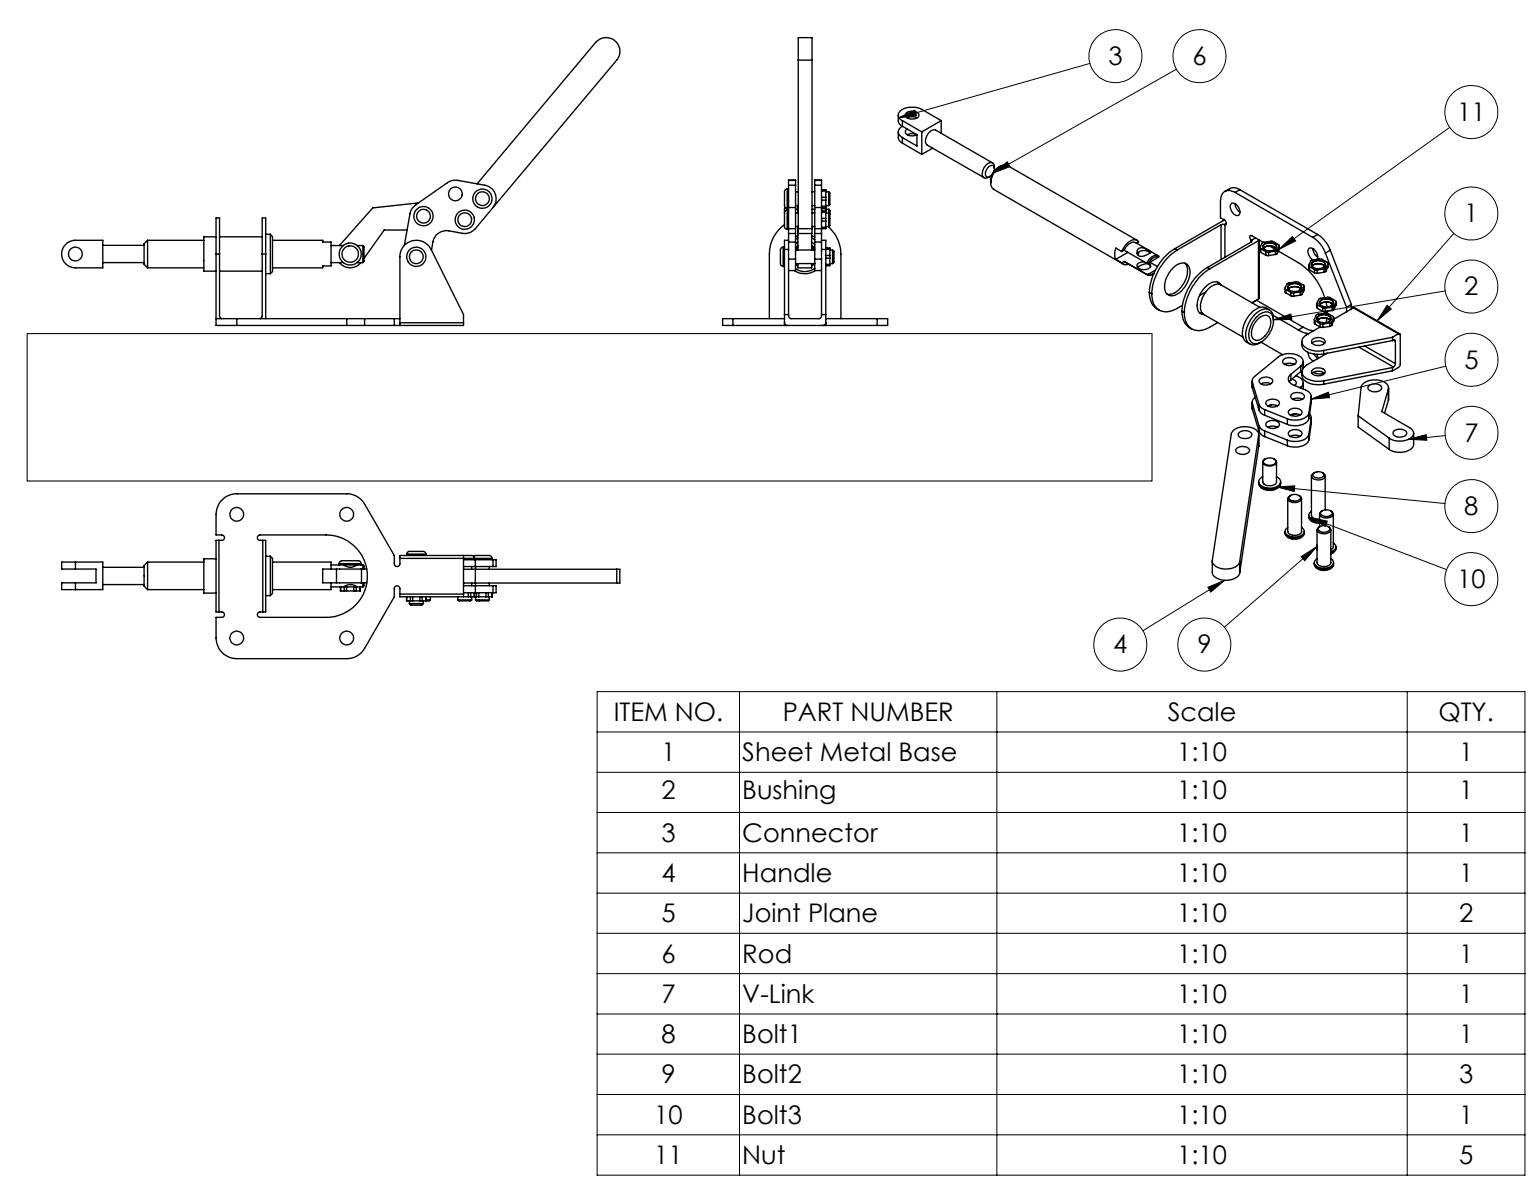
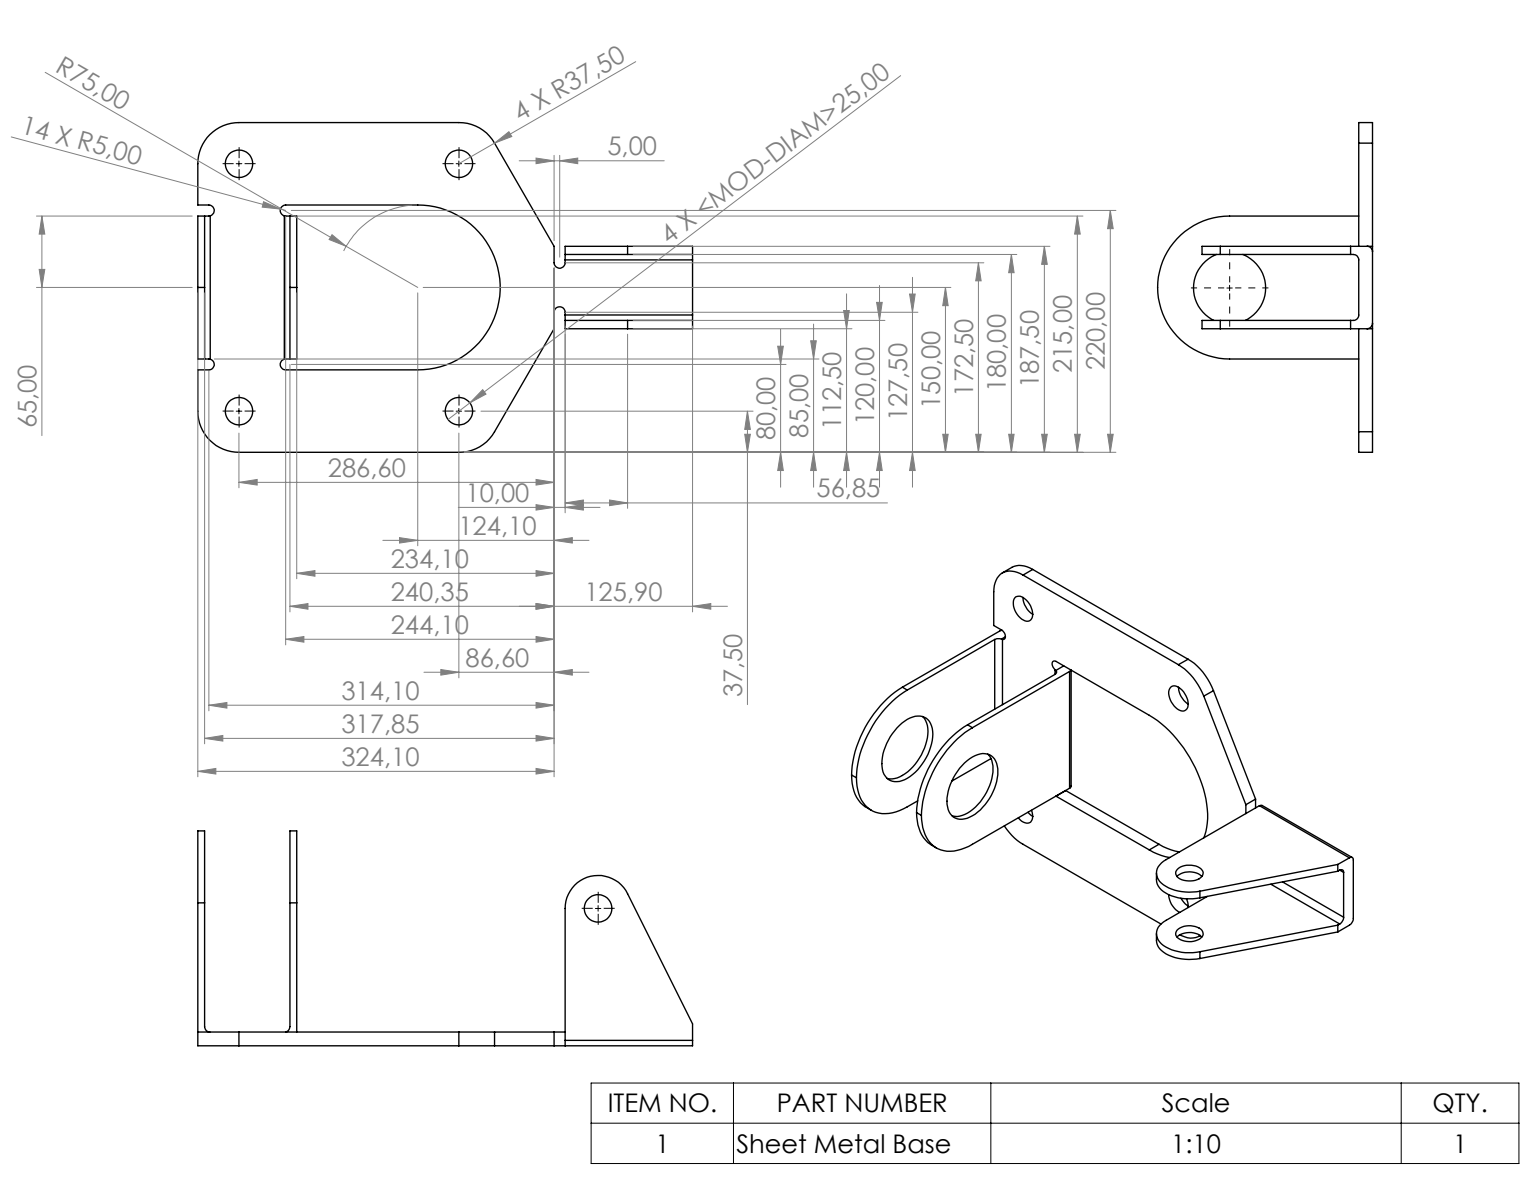
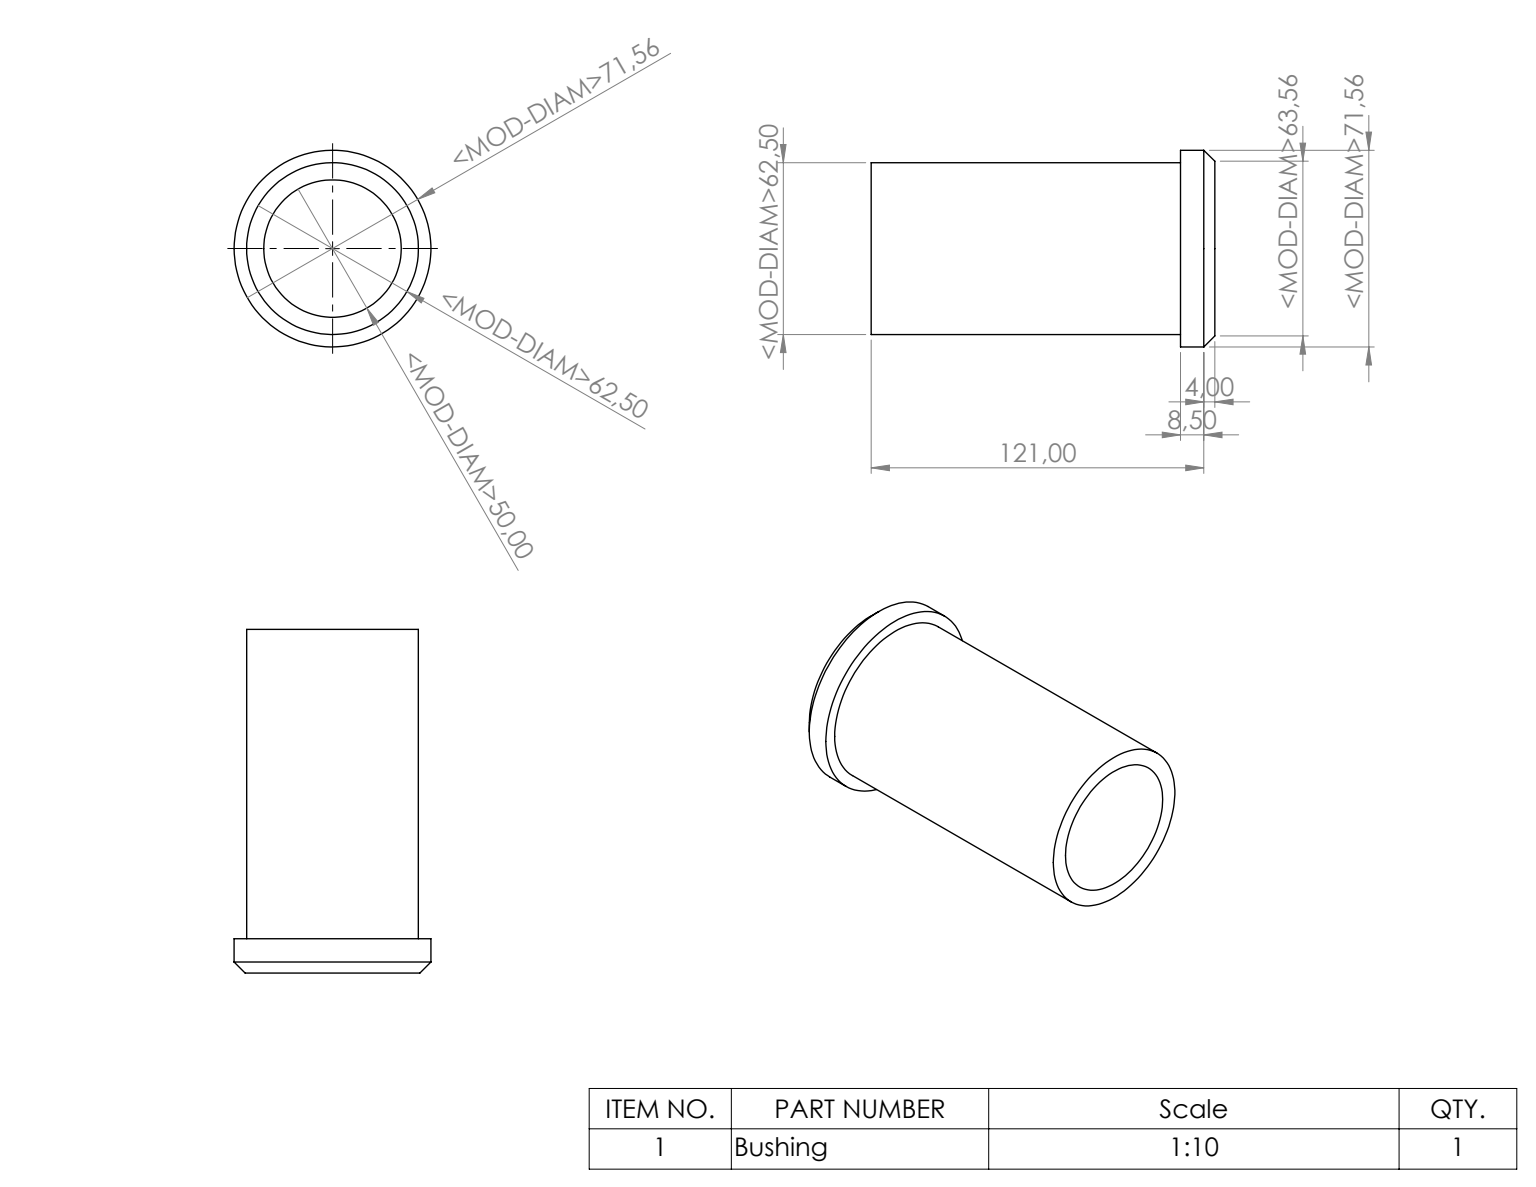
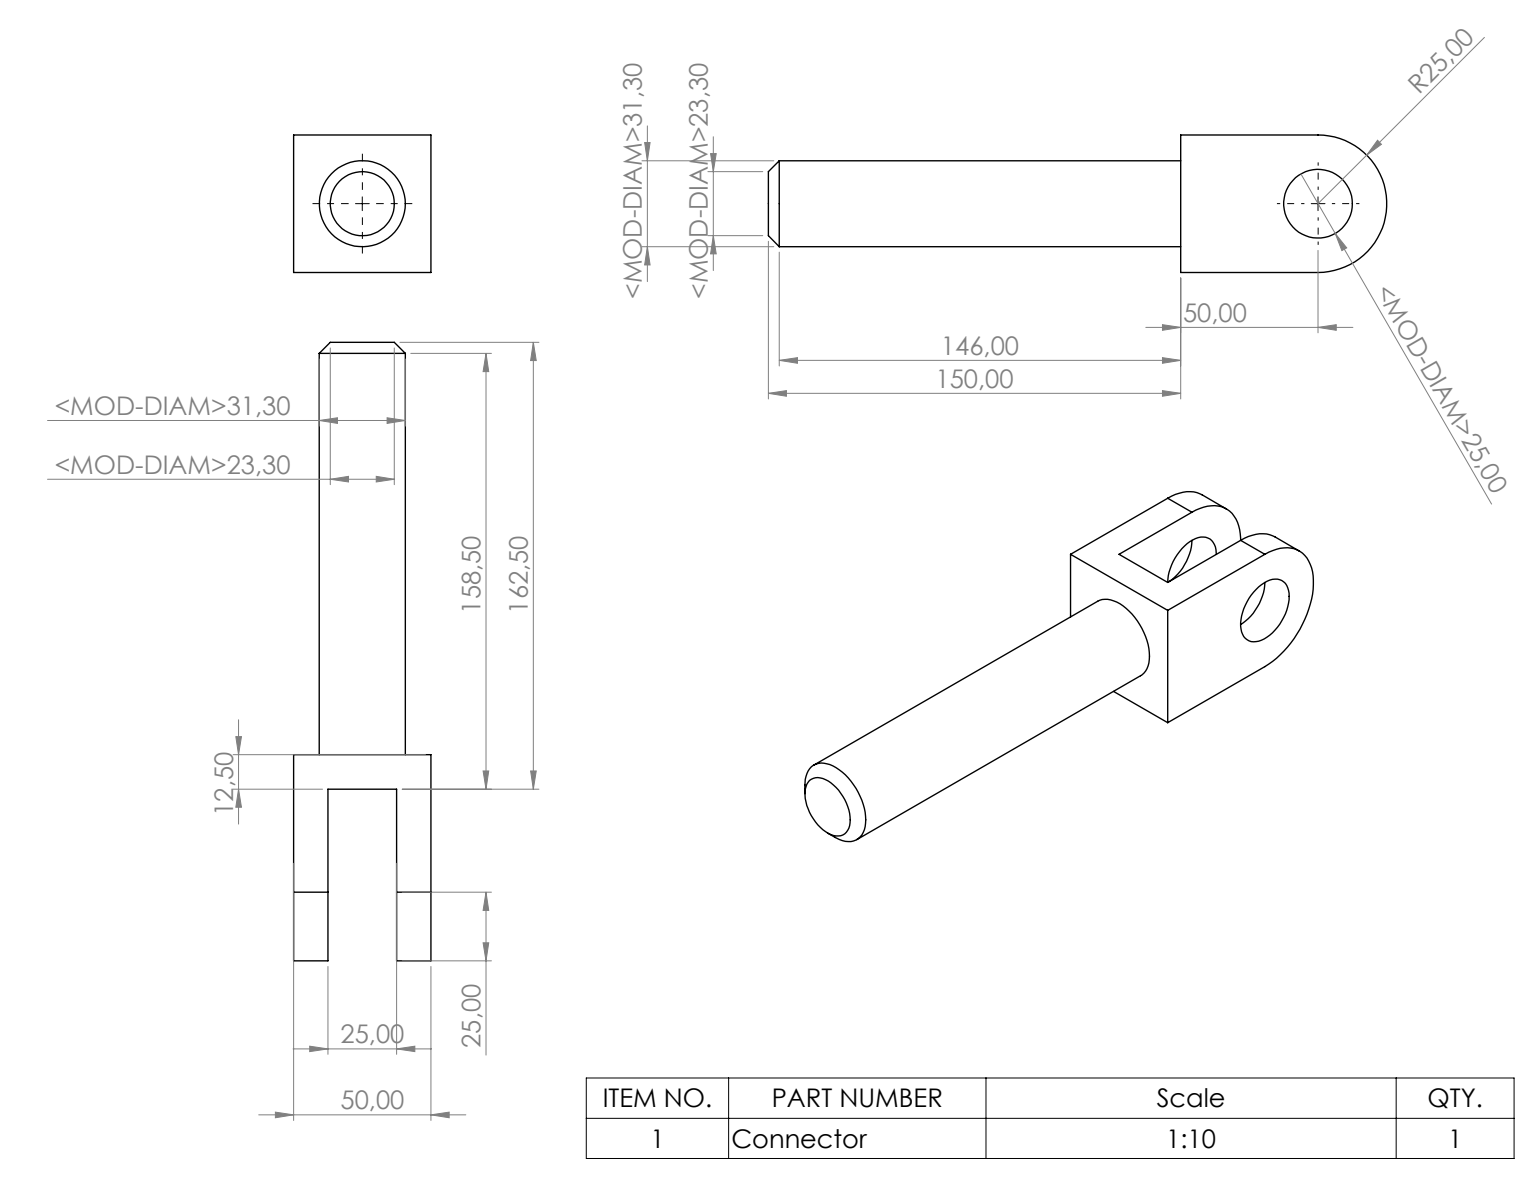
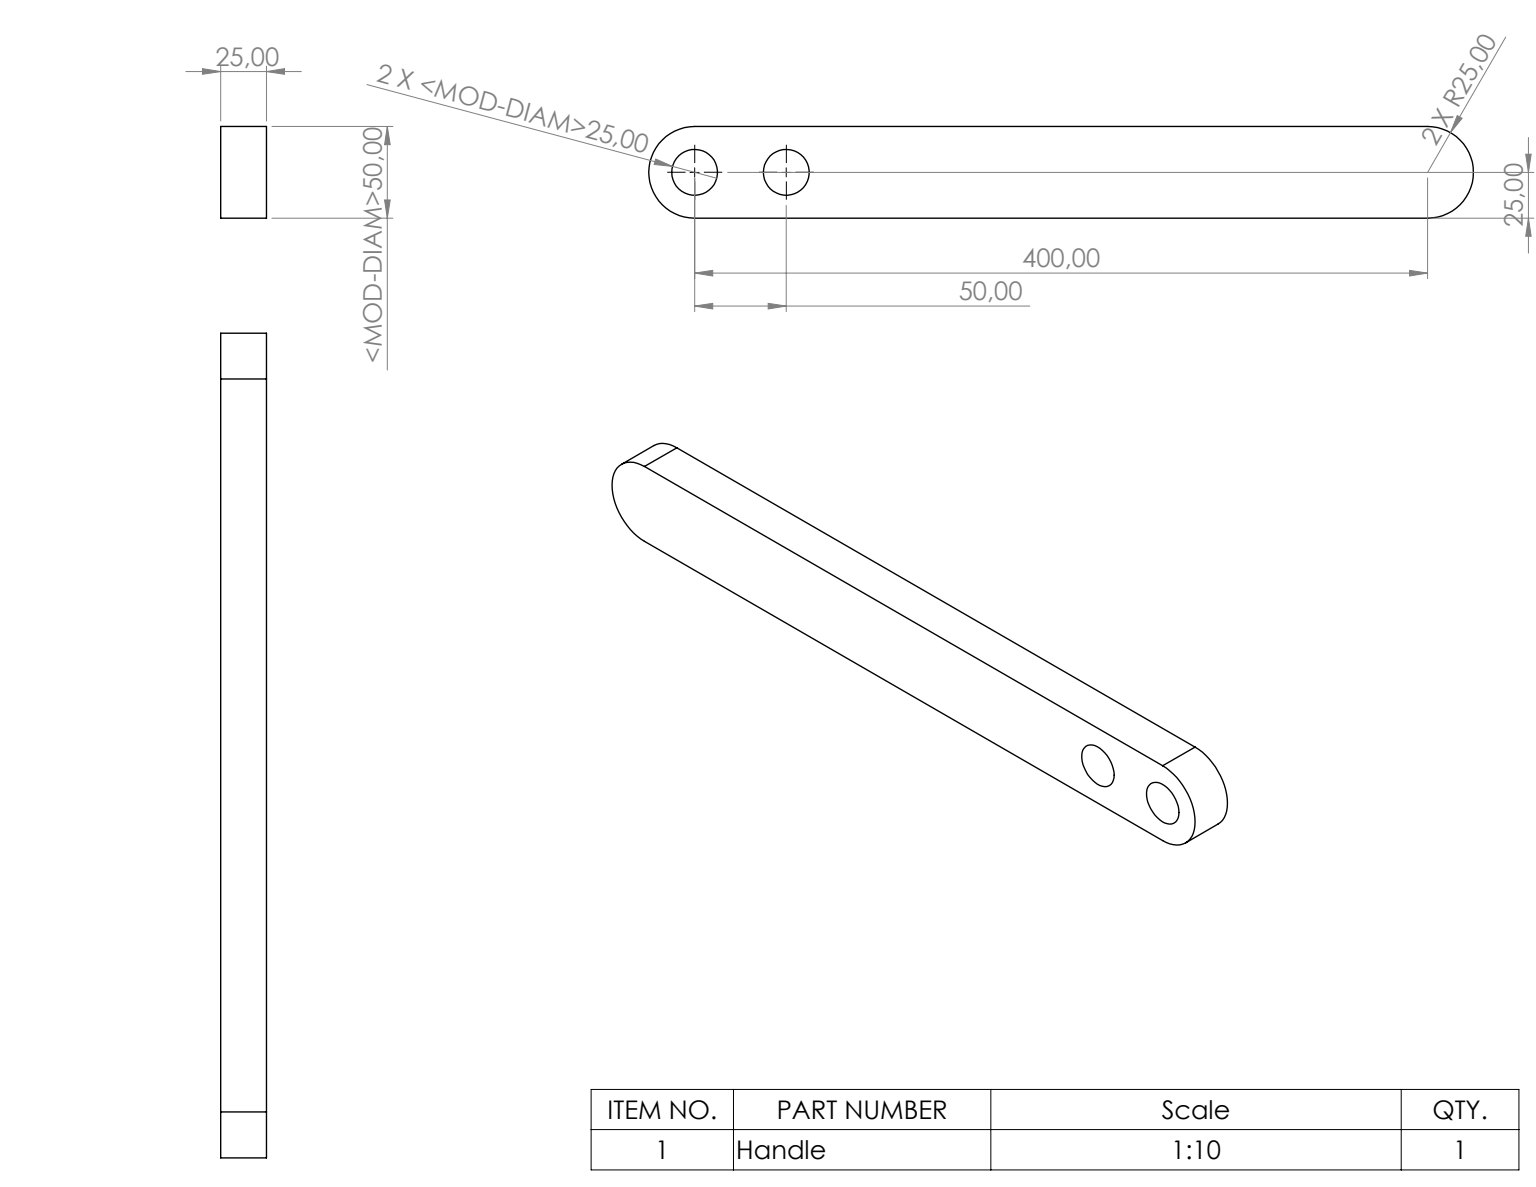
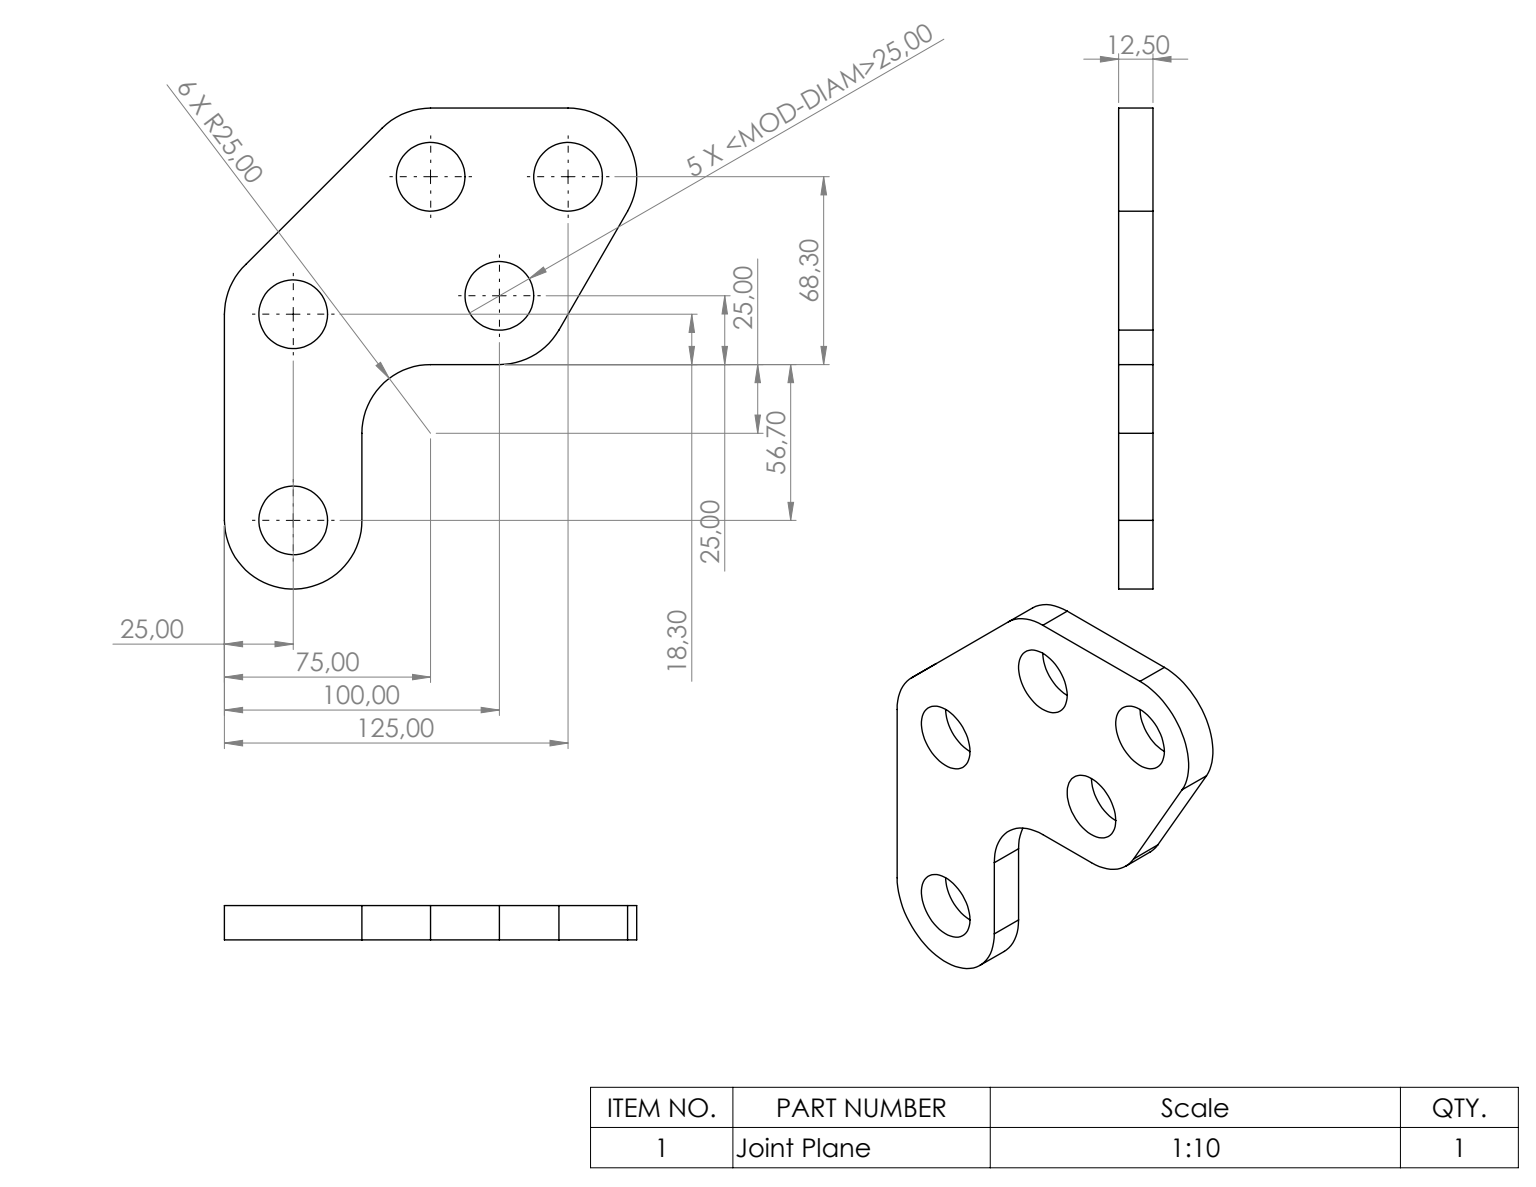
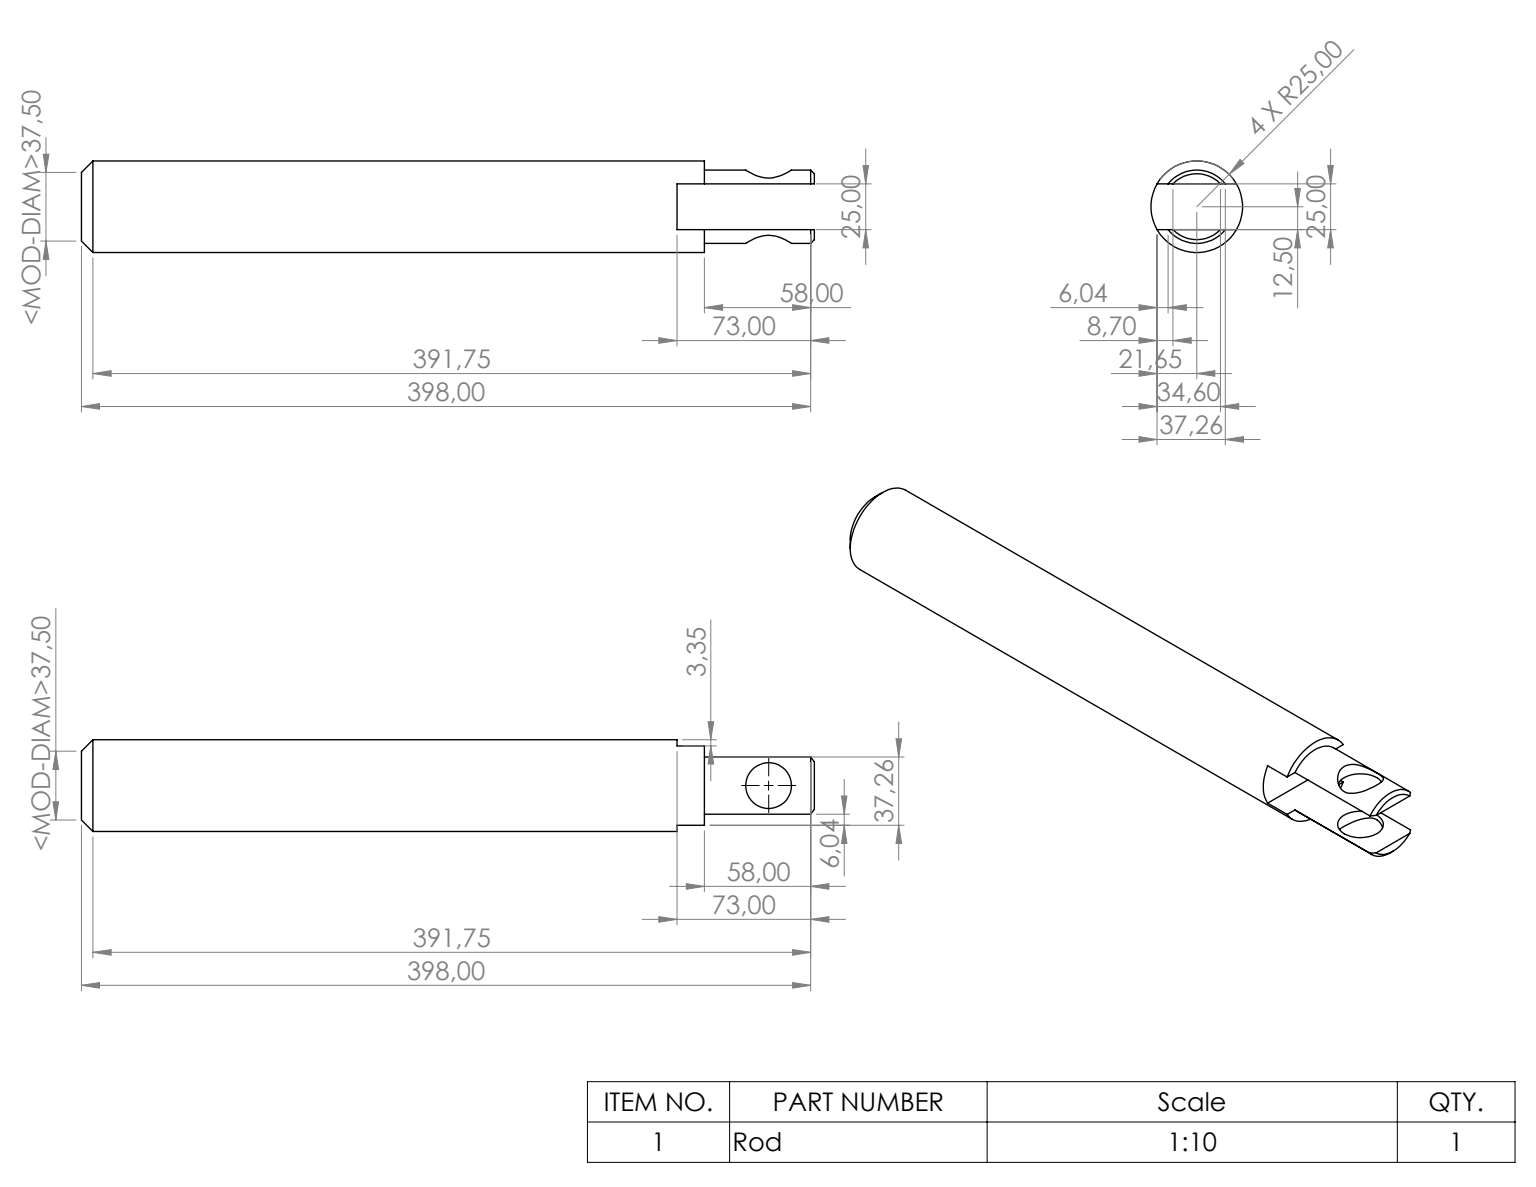
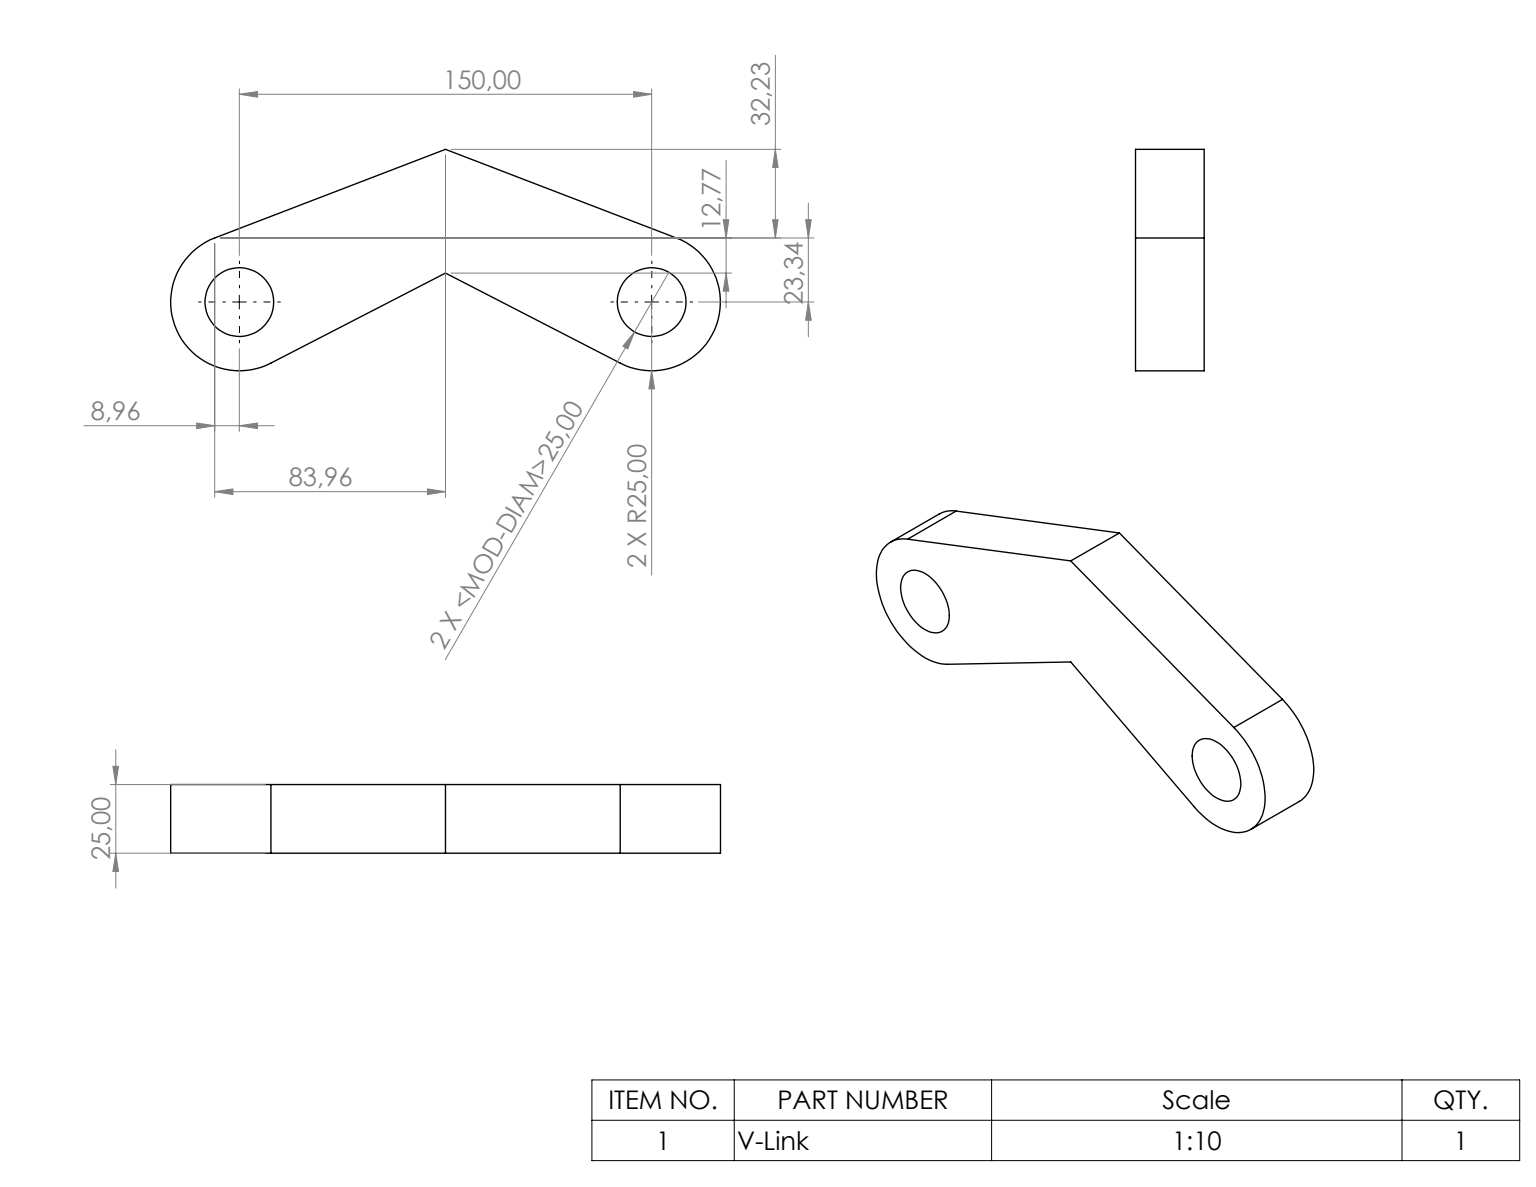
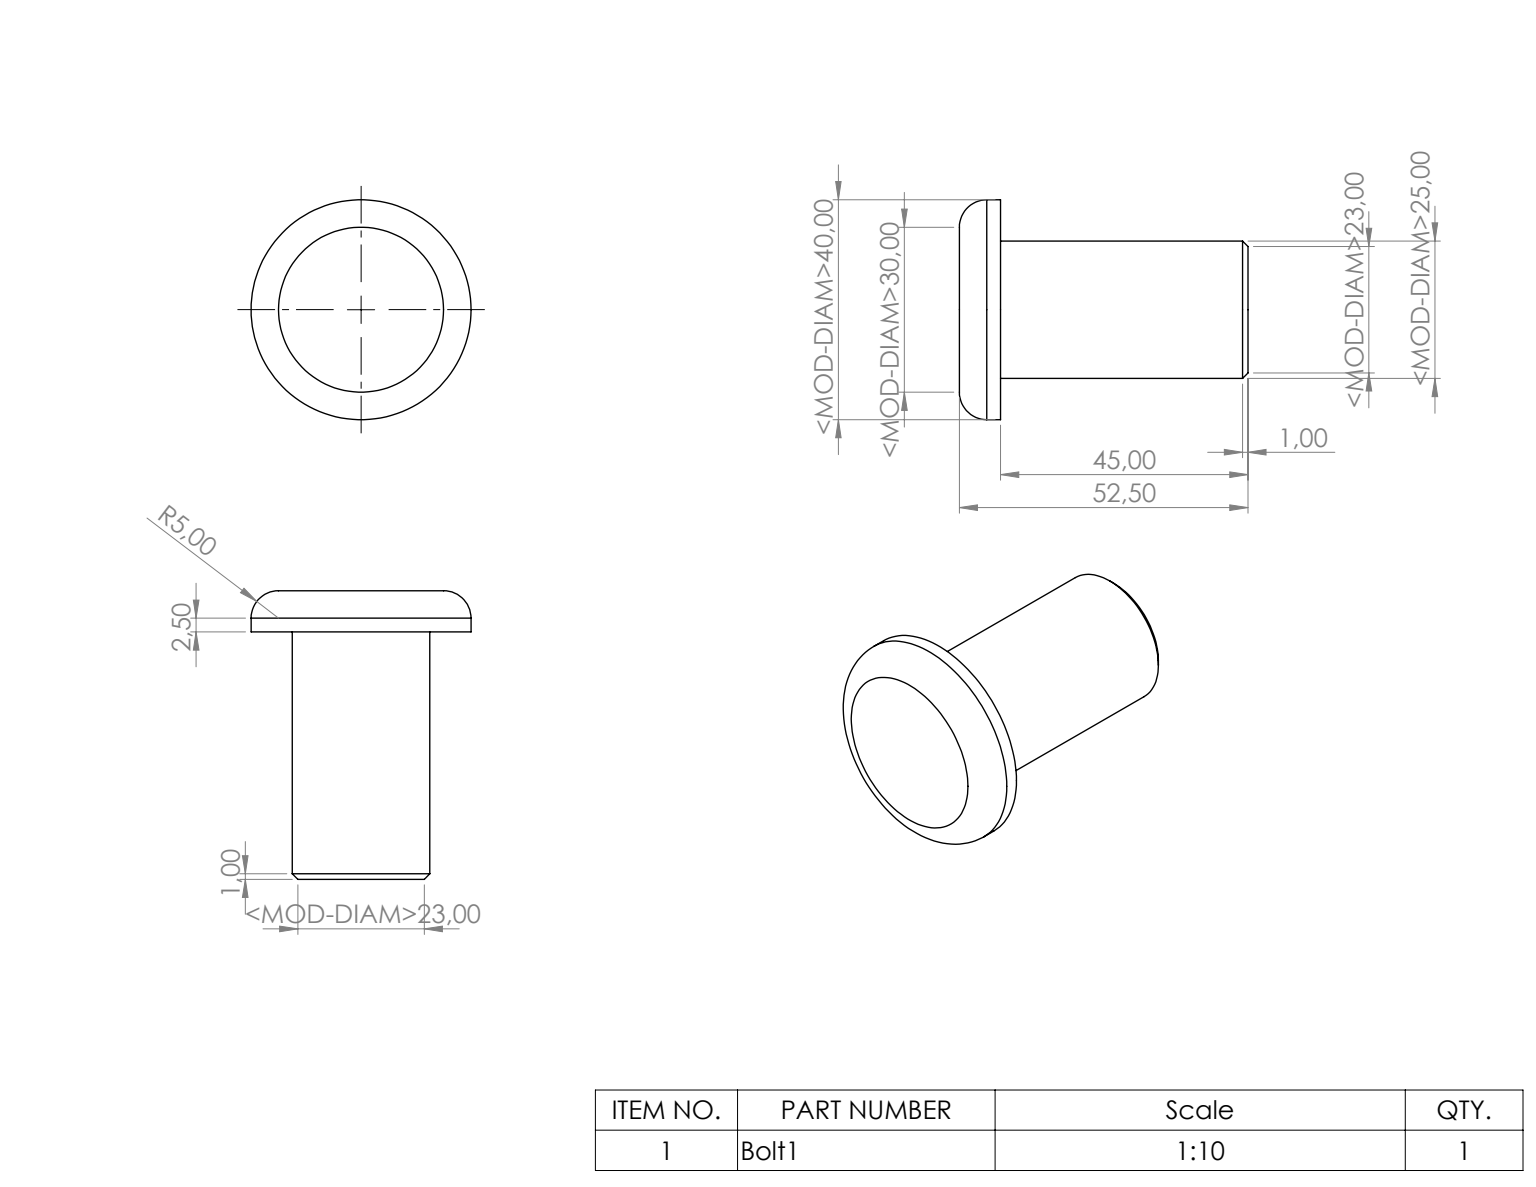
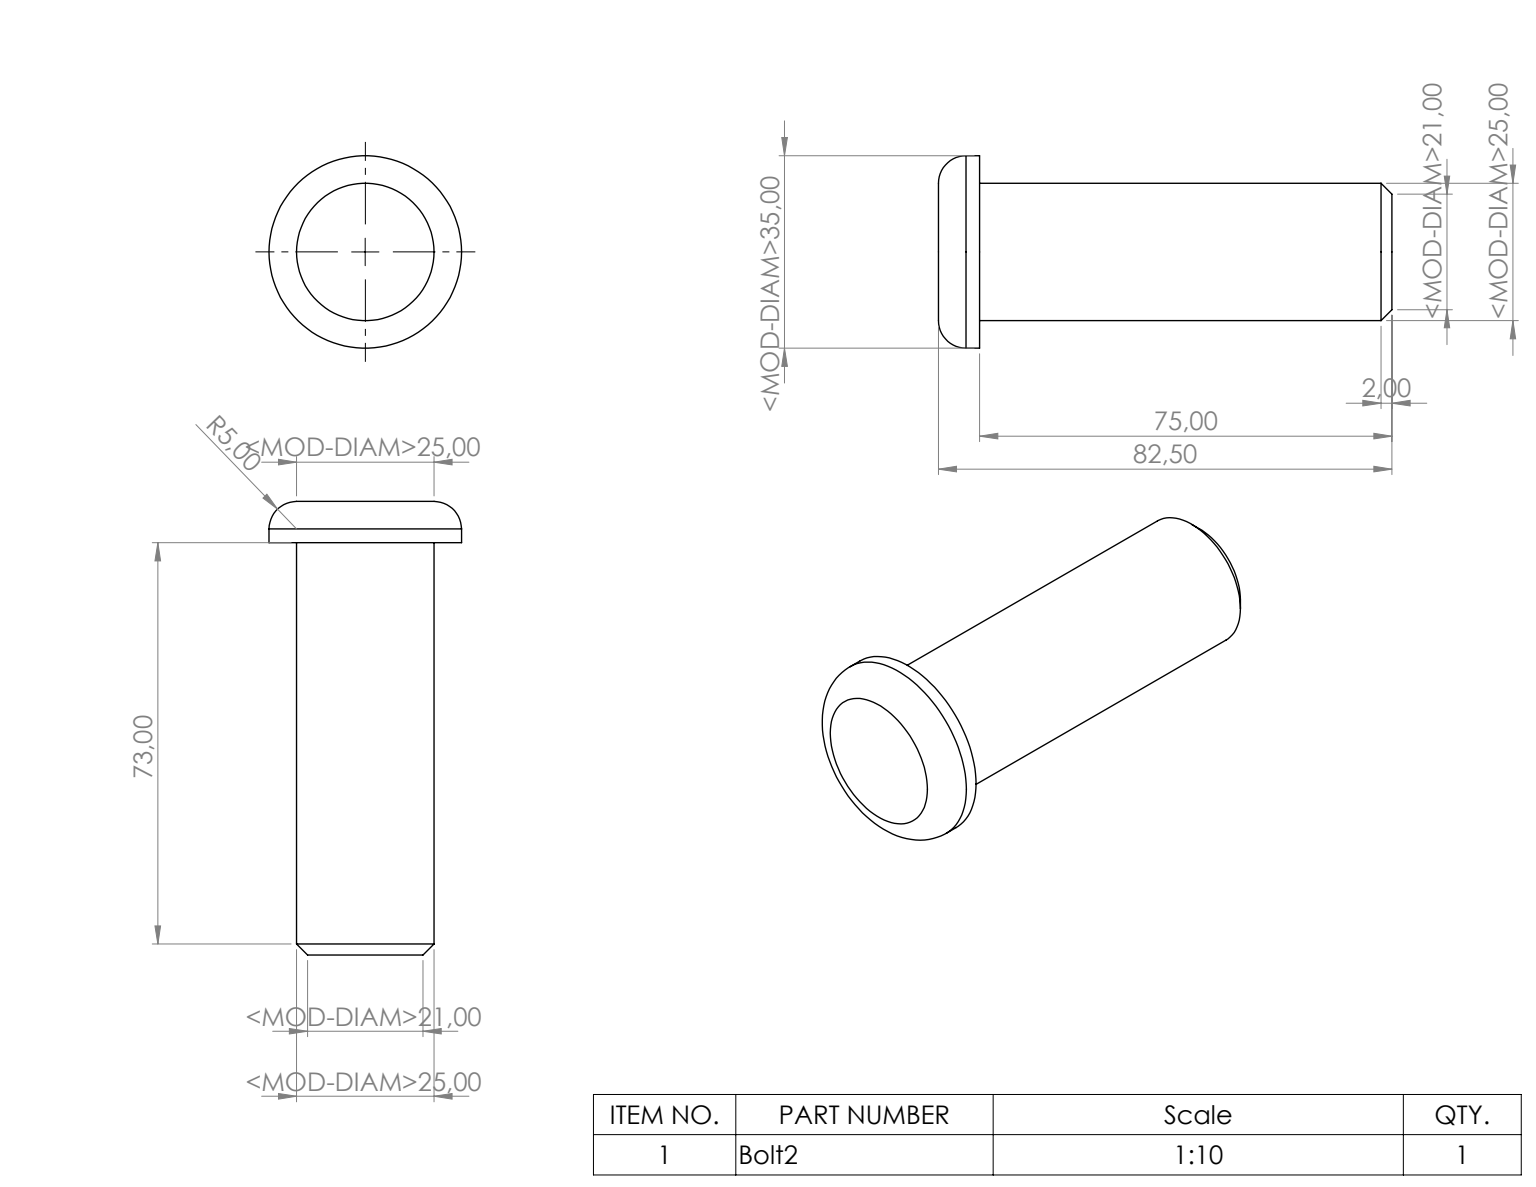
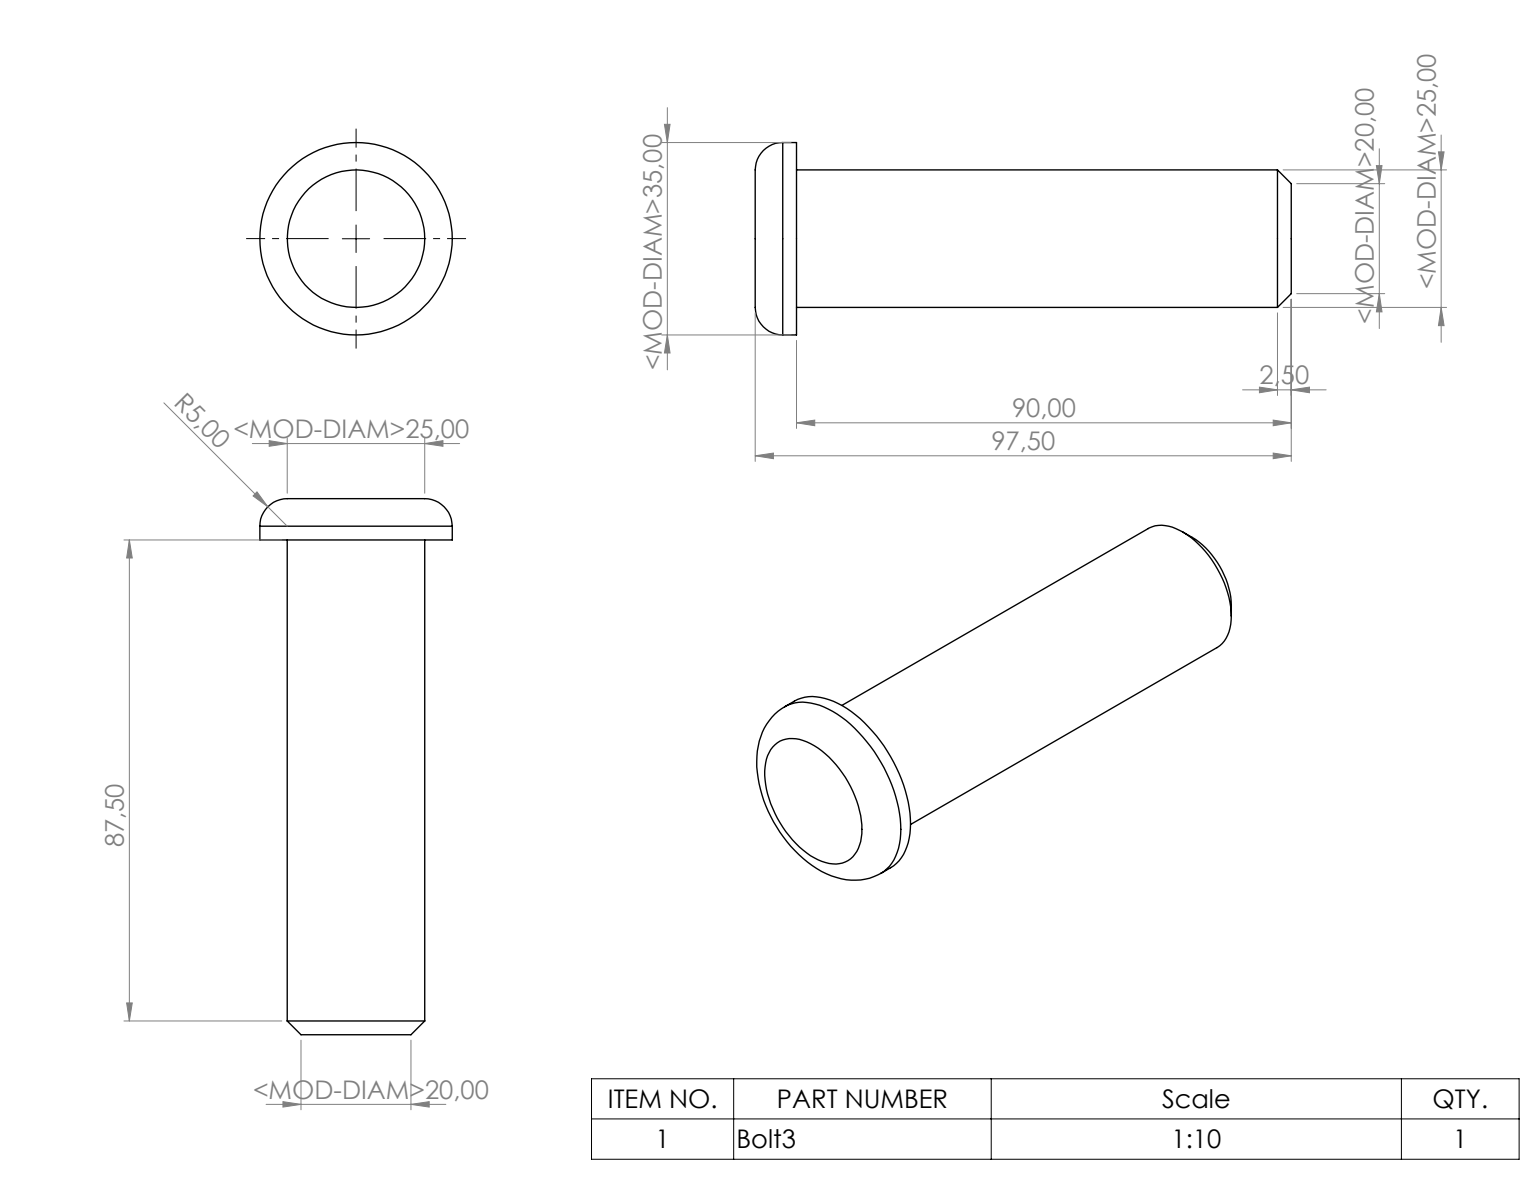
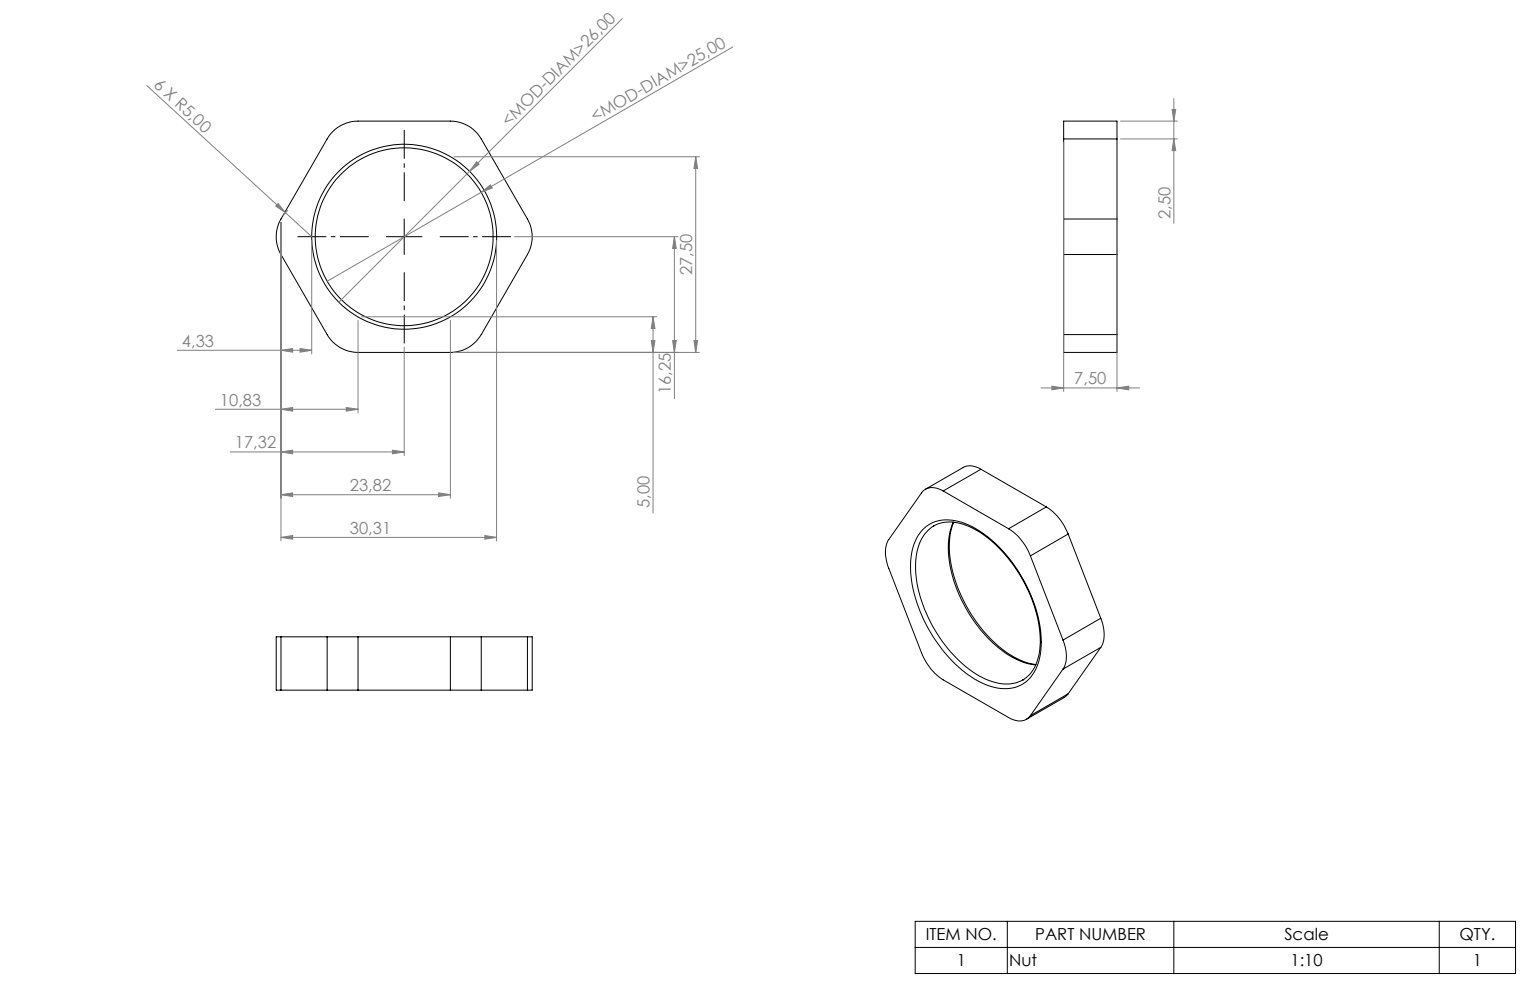
ISO-10303-21;
HEADER;
FILE_DESCRIPTION (('STEP AP214'),
    '1' );
FILE_NAME ('MAT-014',
    '2026-10-28T16:39:03',
    ( '' ),
    ( '' ),
    'SwSTEP 2.0',
    'SolidWorks 2024',
    '' );
FILE_SCHEMA (( 'AUTOMOTIVE_DESIGN' ));
ENDSEC;

DATA;
#1 = VERTEX_POINT ( 'NONE', #6487 ) ;
#2 = VERTEX_POINT ( 'NONE', #3957 ) ;
#3 = CARTESIAN_POINT ( 'NONE',  ( 375.4247212639274380, -15.61249499599598956, 12.50000000000000533 ) ) ;
#4 = ADVANCED_FACE ( 'NONE', ( #7050 ), #2111, .F. ) ;
#5 = LINE ( 'NONE', #7463, #3697 ) ;
#6 = DIRECTION ( 'NONE',  ( 1.000000000000000000, 0.000000000000000000, 0.000000000000000000 ) ) ;
#7 = LINE ( 'NONE', #3105, #4260 ) ;
#8 = CARTESIAN_POINT ( 'NONE',  ( 3.081487911019577803E-31, -25.00000000000000355, 37.50000000000000000 ) ) ;
#9 = CARTESIAN_POINT ( 'NONE',  ( 387.3898630172379285, 19.93132096080314497, 1.708129828930195826 ) ) ;
#10 = ADVANCED_BREP_SHAPE_REPRESENTATION ( '', ( #4174, #5785 ), #5126 ) ;
#11 = LINE ( 'NONE', #7275, #2680 ) ;
#12 = AXIS2_PLACEMENT_3D ( 'NONE', #2676, #866, #3439 ) ;
#13 = DIRECTION ( 'NONE',  ( -1.000000000000000000, -0.000000000000000000, -0.000000000000000000 ) ) ;
#14 = CARTESIAN_POINT ( 'NONE',  ( -12.99038105676657651, 1.734723475976807094E-15, 0.000000000000000000 ) ) ;
#15 = CARTESIAN_POINT ( 'NONE',  ( 199.9999999999998863, 262.5000000000000568, 0.000000000000000000 ) ) ;
#16 = AXIS2_PLACEMENT_3D ( 'NONE', #4137, #1054, #5872 ) ;
#17 = ORIENTED_EDGE ( 'NONE', *, *, #7884, .F. ) ;
#18 = ORIENTED_EDGE ( 'NONE', *, *, #3876, .T. ) ;
#19 = LINE ( 'NONE', #1821, #4426 ) ;
#20 = DIRECTION ( 'NONE',  ( 1.000000000000000000, 0.000000000000000000, 0.000000000000000000 ) ) ;
#21 = DIRECTION ( 'NONE',  ( 0.000000000000000000, 0.000000000000000000, -1.000000000000000000 ) ) ;
#22 = EDGE_LOOP ( 'NONE', ( #4827, #5476, #5226, #672 ) ) ;
#23 = CARTESIAN_POINT ( 'NONE',  ( -74.28095588234631919, 12.70544120911856112, 12.50000000000000000 ) ) ;
#24 = ADVANCED_FACE ( 'NONE', ( #907 ), #1513, .T. ) ;
#25 = ORIENTED_EDGE ( 'NONE', *, *, #6041, .T. ) ;
#26 = ADVANCED_FACE ( 'NONE', ( #6325 ), #4629, .T. ) ;
#27 = CARTESIAN_POINT ( 'NONE',  ( 371.6961001703501211, 15.95358756117676258, -12.06260739558933714 ) ) ;
#28 = VERTEX_POINT ( 'NONE', #2799 ) ;
#29 = CARTESIAN_POINT ( 'NONE',  ( 368.6956339375703351, -16.83403191367835561, 10.80131548116625417 ) ) ;
#30 = VERTEX_POINT ( 'NONE', #1471 ) ;
#31 = LINE ( 'NONE', #3054, #2794 ) ;
#32 = DIRECTION ( 'NONE',  ( 1.000000000000000000, 0.000000000000000000, 0.000000000000000000 ) ) ;
#33 = EDGE_CURVE ( 'NONE', #7631, #7527, #437, .T. ) ;
#34 = ORIENTED_EDGE ( 'NONE', *, *, #3876, .F. ) ;
#35 = EDGE_LOOP ( 'NONE', ( #6541, #2279, #2364, #4470, #5618 ) ) ;
#36 = VERTEX_POINT ( 'NONE', #5235 ) ;
#37 = CARTESIAN_POINT ( 'NONE',  ( 376.6870407283136046, -15.69785030319133945, 12.39275847443047773 ) ) ;
#38 = CARTESIAN_POINT ( 'NONE',  ( 0.000000000000000000, 0.000000000000000000, 75.00000000000000000 ) ) ;
#39 = DIRECTION ( 'NONE',  ( 1.000000000000000000, 0.000000000000000000, 0.000000000000000000 ) ) ;
#40 = LINE ( 'NONE', #6225, #5683 ) ;
#41 = DIRECTION ( 'NONE',  ( 0.000000000000000000, -1.000000000000000000, 0.000000000000000000 ) ) ;
#42 = CIRCLE ( 'NONE', #1071, 15.64999999999999680 ) ;
#43 = EDGE_CURVE ( 'NONE', #2392, #5200, #812, .T. ) ;
#44 = VECTOR ( 'NONE', #6723, 1000.000000000000000 ) ;
#45 = AXIS2_PLACEMENT_3D ( 'NONE', #6354, #218, #7634 ) ;
#46 = DIRECTION ( 'NONE',  ( 0.7071067811865502373, 0.000000000000000000, 0.7071067811865447972 ) ) ;
#47 = CARTESIAN_POINT ( 'NONE',  ( -24.28095581706361727, -30.59582894744887582, 0.000000000000000000 ) ) ;
#48 = FACE_OUTER_BOUND ( 'NONE', #2158, .T. ) ;
#49 = DIRECTION ( 'NONE',  ( 0.000000000000000000, 0.000000000000000000, 1.000000000000000000 ) ) ;
#50 = AXIS2_PLACEMENT_3D ( 'NONE', #3727, #3599, #6048 ) ;
#51 = AXIS2_PLACEMENT_3D ( 'NONE', #3862, #3896, #3257 ) ;
#52 = VERTEX_POINT ( 'NONE', #7725 ) ;
#53 = ORIENTED_EDGE ( 'NONE', *, *, #7404, .F. ) ;
#54 = LINE ( 'NONE', #4948, #4837 ) ;
#56 = CARTESIAN_POINT ( 'NONE',  ( 0.7190441502950353225, 87.70544117646394966, 0.000000000000000000 ) ) ;
#55 = CIRCLE ( 'NONE', #4287, 65.50000000000000000 ) ;
#57 = AXIS2_PLACEMENT_3D ( 'NONE', #6318, #3273, #5723 ) ;
#58 = DIRECTION ( 'NONE',  ( 1.000000000000000000, 0.000000000000000000, 0.000000000000000000 ) ) ;
#59 = ORIENTED_EDGE ( 'NONE', *, *, #2376, .F. ) ;
#60 = DIRECTION ( 'NONE',  ( 0.000000000000000000, -0.000000000000000000, 1.000000000000000000 ) ) ;
#61 = ADVANCED_FACE ( 'NONE', ( #3280, #3358 ), #6366, .T. ) ;
#62 = AXIS2_PLACEMENT_3D ( 'NONE', #1310, #5647, #5485 ) ;
#63 = ORIENTED_EDGE ( 'NONE', *, *, #3507, .F. ) ;
#64 = CARTESIAN_POINT ( 'NONE',  ( 370.5187250548066231, 16.23897639391231706, -11.67616422689687639 ) ) ;
#65 = ORIENTED_EDGE ( 'NONE', *, *, #7166, .T. ) ;
#66 = CARTESIAN_POINT ( 'NONE',  ( 364.2065580935995968, -18.97653311414304511, 6.355249004872655760 ) ) ;
#67 = ORIENTED_EDGE ( 'NONE', *, *, #5175, .F. ) ;
#68 = EDGE_CURVE ( 'NONE', #6240, #2057, #7224, .T. ) ;
#69 = CARTESIAN_POINT ( 'NONE',  ( 0.000000000000000000, 0.000000000000000000, 0.000000000000000000 ) ) ;
#70 = VECTOR ( 'NONE', #486, 999.9999999999998863 ) ;
#71 = DIRECTION ( 'NONE',  ( -0.000000000000000000, -0.000000000000000000, -1.000000000000000000 ) ) ;
#72 = EDGE_CURVE ( 'NONE', #4343, #3684, #1276, .T. ) ;
#73 = ORIENTED_EDGE ( 'NONE', *, *, #3667, .F. ) ;
#74 = ORIENTED_EDGE ( 'NONE', *, *, #3629, .F. ) ;
#75 = B_SPLINE_CURVE_WITH_KNOTS ( 'NONE', 3,
 ( #2455, #1205, #4890, #7349 ),
 .UNSPECIFIED., .F., .F.,
 ( 4, 4 ),
 ( 0.000000000000000000, 0.001270006434950045771 ),
 .UNSPECIFIED. ) ;
#76 = EDGE_CURVE ( 'NONE', #6360, #3593, #5967, .T. ) ;
#77 = ORIENTED_EDGE ( 'NONE', *, *, #5334, .F. ) ;
#78 = CARTESIAN_POINT ( 'NONE',  ( 1.320471425210250835E-15, 0.000000000000000000, 0.000000000000000000 ) ) ;
#79 = ADVANCED_FACE ( 'NONE', ( #5146 ), #2881, .F. ) ;
#80 = LINE ( 'NONE', #2529, #4060 ) ;
#81 = CARTESIAN_POINT ( 'NONE',  ( 279.9038105676658006, 161.6025403784438765, 0.000000000000000000 ) ) ;
#82 = FACE_OUTER_BOUND ( 'NONE', #3199, .T. ) ;
#83 = CARTESIAN_POINT ( 'NONE',  ( 25.71904415029483459, 19.40417101989674009, 12.50000000000000000 ) ) ;
#84 = PRESENTATION_LAYER_ASSIGNMENT (  '', '', ( #3420 ) ) ;
#85 = EDGE_CURVE ( 'NONE', #4850, #1396, #297, .T. ) ;
#86 = VECTOR ( 'NONE', #7226, 1000.000000000000000 ) ;
#87 = SHAPE_DEFINITION_REPRESENTATION ( #2063, #2908 ) ;
#88 = CARTESIAN_POINT ( 'NONE',  ( 47.36967921662626679, 6.904171036223937463, 0.000000000000000000 ) ) ;
#89 = DIRECTION ( 'NONE',  ( -0.000000000000000000, -0.000000000000000000, -1.000000000000000000 ) ) ;
#90 = DIRECTION ( 'NONE',  ( -0.000000000000000000, -0.000000000000000000, -1.000000000000000000 ) ) ;
#91 = CYLINDRICAL_SURFACE ( 'NONE', #5688, 5.000000000000004441 ) ;
#92 = CIRCLE ( 'NONE', #7022, 0.5000000000000004441 ) ;
#93 = EDGE_LOOP ( 'NONE', ( #2797, #6100, #4748, #419 ) ) ;
#94 =( LENGTH_UNIT ( ) NAMED_UNIT ( * ) SI_UNIT ( .MILLI., .METRE. ) );
#95 = ORIENTED_EDGE ( 'NONE', *, *, #1155, .F. ) ;
#96 = COLOUR_RGB ( '',0.7921568627450980005, 0.8196078431372548767, 0.9333333333333333481 ) ;
#97 = DIRECTION ( 'NONE',  ( 0.5000000000000000000, 0.8660254037844385966, 0.000000000000000000 ) ) ;
#98 = CYLINDRICAL_SURFACE ( 'NONE', #6896, 12.50000000000001066 ) ;
#99 = CIRCLE ( 'NONE', #3701, 12.50000000000001066 ) ;
#100 = PLANE ( 'NONE',  #441 ) ;
#101 = EDGE_CURVE ( 'NONE', #792, #1942, #1186, .T. ) ;
#102 = FACE_OUTER_BOUND ( 'NONE', #3804, .T. ) ;
#103 = VERTEX_POINT ( 'NONE', #2394 ) ;
#104 = CARTESIAN_POINT ( 'NONE',  ( 0.000000000000000000, 187.5000000000000000, 0.000000000000000000 ) ) ;
#105 = VECTOR ( 'NONE', #3844, 1000.000000000000000 ) ;
#106 = VECTOR ( 'NONE', #6998, 1000.000000000000000 ) ;
#107 = VERTEX_POINT ( 'NONE', #1630 ) ;
#108 = LINE ( 'NONE', #6772, #1142 ) ;
#109 = VERTEX_POINT ( 'NONE', #3635 ) ;
#110 = CARTESIAN_POINT ( 'NONE',  ( -13.00000000000000178, 1.592040838891559293E-15, 7.500000000000000000 ) ) ;
#111 = ORIENTED_EDGE ( 'NONE', *, *, #2037, .T. ) ;
#112 = VECTOR ( 'NONE', #5302, 1000.000000000000000 ) ;
#113 = DIRECTION ( 'NONE',  ( 0.000000000000000000, 0.000000000000000000, 1.000000000000000000 ) ) ;
#114 = AXIS2_PLACEMENT_3D ( 'NONE', #4743, #7238, #7119 ) ;
#115 = LINE ( 'NONE', #7340, #7495 ) ;
#116 = VERTEX_POINT ( 'NONE', #2354 ) ;
#117 = VECTOR ( 'NONE', #1190, 1000.000000000000000 ) ;
#118 = CIRCLE ( 'NONE', #4338, 5.000000000000000888 ) ;
#119 = EDGE_LOOP ( 'NONE', ( #1348, #4627 ) ) ;
#120 = ORIENTED_EDGE ( 'NONE', *, *, #43, .F. ) ;
#121 = CARTESIAN_POINT ( 'NONE',  ( 10.82531754730547213, 13.75000000000000178, 7.500000000000000000 ) ) ;
#122 = CARTESIAN_POINT ( 'NONE',  ( 375.8519756245596568, -15.61249499599599311, -12.50000000000000000 ) ) ;
#123 = DIRECTION ( 'NONE',  ( 1.000000000000000000, 0.000000000000000000, 0.000000000000000000 ) ) ;
#124 = DIRECTION ( 'NONE',  ( -1.000000000000000000, 0.000000000000000000, 0.000000000000000000 ) ) ;
#125 = CYLINDRICAL_SURFACE ( 'NONE', #7742, 12.50000000000000000 ) ;
#126 = EDGE_CURVE ( 'NONE', #36, #6483, #6084, .T. ) ;
#127 = EDGE_CURVE ( 'NONE', #5728, #5686, #5812, .T. ) ;
#128 = CONTEXT_DEPENDENT_SHAPE_REPRESENTATION ( #3628, #4558 ) ;
#129 = CARTESIAN_POINT ( 'NONE',  ( 42.50000000000000000, 42.50000000000003553, 12.50000000000000000 ) ) ;
#130 = CARTESIAN_POINT ( 'NONE',  ( 72.36967921662629522, 50.20544122544588816, 12.50000000000000000 ) ) ;
#131 = LINE ( 'NONE', #1259, #5311 ) ;
#132 = CARTESIAN_POINT ( 'NONE',  ( 125.0000000000000000, 0.000000000000000000, 0.000000000000000000 ) ) ;
#133 = APPLICATION_CONTEXT ( 'automotive_design' ) ;
#134 = EDGE_CURVE ( 'NONE', #6179, #1386, #5939, .T. ) ;
#135 = ADVANCED_FACE ( 'NONE', ( #1032 ), #5362, .T. ) ;
#136 = VERTEX_POINT ( 'NONE', #4752 ) ;
#137 = CARTESIAN_POINT ( 'NONE',  ( 6.495190528383280260, 11.25000000000000000, 7.500000000000000000 ) ) ;
#138 = ORIENTED_EDGE ( 'NONE', *, *, #4119, .T. ) ;
#139 = CYLINDRICAL_SURFACE ( 'NONE', #3161, 24.99999999999999289 ) ;
#140 = DIRECTION ( 'NONE',  ( -0.000000000000000000, -0.000000000000000000, -1.000000000000000000 ) ) ;
#141 = DIRECTION ( 'NONE',  ( -0.000000000000000000, 0.000000000000000000, 1.000000000000000000 ) ) ;
#142 = CARTESIAN_POINT ( 'NONE',  ( -31.24999999999997158, 111.9999999999999289, 130.0000000000000000 ) ) ;
#143 = ORIENTED_EDGE ( 'NONE', *, *, #3611, .T. ) ;
#144 = VECTOR ( 'NONE', #7565, 1000.000000000000000 ) ;
#145 = DIRECTION ( 'NONE',  ( -0.000000000000000000, -0.000000000000000000, -1.000000000000000000 ) ) ;
#146 = VECTOR ( 'NONE', #1608, 1000.000000000000000 ) ;
#147 = EDGE_CURVE ( 'NONE', #3810, #7620, #42, .T. ) ;
#148 = CARTESIAN_POINT ( 'NONE',  ( 362.5886599408613051, 19.94427247194493802, -1.702902647306309358 ) ) ;
#150 = VERTEX_POINT ( 'NONE', #4789 ) ;
#149 = AXIS2_PLACEMENT_3D ( 'NONE', #2056, #4502, #6954 ) ;
#151 = DIRECTION ( 'NONE',  ( 0.000000000000000000, 0.000000000000000000, 1.000000000000000000 ) ) ;
#152 = ORIENTED_EDGE ( 'NONE', *, *, #6160, .T. ) ;
#153 = CARTESIAN_POINT ( 'NONE',  ( 0.000000000000000000, 15.00000000000000000, 0.000000000000000000 ) ) ;
#154 = CARTESIAN_POINT ( 'NONE',  ( 138.5360707071662887, -22.21662272193747256, 0.000000000000000000 ) ) ;
#155 = VERTEX_POINT ( 'NONE', #3519 ) ;
#156 = DIRECTION ( 'NONE',  ( 1.000000000000000000, 0.000000000000000000, 0.000000000000000000 ) ) ;
#157 = ORIENTED_EDGE ( 'NONE', *, *, #2928, .F. ) ;
#158 = ORIENTED_EDGE ( 'NONE', *, *, #3995, .T. ) ;
#159 = CYLINDRICAL_SURFACE ( 'NONE', #2014, 12.50000000000000355 ) ;
#160 = CARTESIAN_POINT ( 'NONE',  ( 376.6830312554756688, -15.68244000841234964, -12.41390036673199759 ) ) ;
#161 = VERTEX_POINT ( 'NONE', #6006 ) ;
#162 = CARTESIAN_POINT ( 'NONE',  ( -25.00000000000000711, 0.000000000000000000, 0.000000000000000000 ) ) ;
#163 = CARTESIAN_POINT ( 'NONE',  ( 412.5000000000001137, 1.530808498934191127E-15, 0.000000000000000000 ) ) ;
#164 = CARTESIAN_POINT ( 'NONE',  ( 42.50000000000000711, 182.5000000000000000, 12.50000000000000000 ) ) ;
#165 = DIRECTION ( 'NONE',  ( 0.000000000000000000, 1.000000000000000000, -0.000000000000000000 ) ) ;
#166 = AXIS2_PLACEMENT_3D ( 'NONE', #651, #3778, #1809 ) ;
#167 = DIRECTION ( 'NONE',  ( -1.000000000000000000, -0.000000000000000000, -0.000000000000000000 ) ) ;
#168 = EDGE_CURVE ( 'NONE', #511, #1117, #6645, .T. ) ;
#169 = ADVANCED_FACE ( 'NONE', ( #7879 ), #5968, .T. ) ;
#170 = ORIENTED_EDGE ( 'NONE', *, *, #6739, .T. ) ;
#171 = DIRECTION ( 'NONE',  ( -0.000000000000000000, 0.000000000000000000, -1.000000000000000000 ) ) ;
#172 = DIRECTION ( 'NONE',  ( -0.6432346663207121340, 3.080497388296852007E-16, -0.7656690956563951822 ) ) ;
#173 = ORIENTED_EDGE ( 'NONE', *, *, #2685, .F. ) ;
#174 = DIRECTION ( 'NONE',  ( 0.5000000000000003331, -0.8660254037844383745, 0.000000000000000000 ) ) ;
#175 = CARTESIAN_POINT ( 'NONE',  ( 37.50000000000000711, 182.5000000000000000, 12.50000000000000000 ) ) ;
#176 = CARTESIAN_POINT ( 'NONE',  ( -9.999999999999896971, 1.377727649040766078E-15, 0.000000000000000000 ) ) ;
#177 = CARTESIAN_POINT ( 'NONE',  ( 62.50000000000007105, 79.24999999999987210, 130.0000000000000000 ) ) ;
#178 = ORIENTED_EDGE ( 'NONE', *, *, #7323, .T. ) ;
#179 = AXIS2_PLACEMENT_3D ( 'NONE', #6550, #500, #1729 ) ;
#180 = AXIS2_PLACEMENT_3D ( 'NONE', #6279, #3725, #665 ) ;
#181 = ORIENTED_EDGE ( 'NONE', *, *, #776, .F. ) ;
#182 = AXIS2_PLACEMENT_3D ( 'NONE', #3889, #3931, #5783 ) ;
#183 = LINE ( 'NONE', #5111, #144 ) ;
#184 = EDGE_LOOP ( 'NONE', ( #4284, #4877, #609, #2812 ) ) ;
#185 = VECTOR ( 'NONE', #4899, 1000.000000000000000 ) ;
#186 = DIRECTION ( 'NONE',  ( 0.5000000000000001110, 0.8660254037844385966, 0.000000000000000000 ) ) ;
#187 = ORIENTED_EDGE ( 'NONE', *, *, #4482, .T. ) ;
#188 = DIRECTION ( 'NONE',  ( -0.000000000000000000, 1.000000000000000000, 1.387778780781445676E-16 ) ) ;
#189 = DIRECTION ( 'NONE',  ( 1.000000000000000000, 0.000000000000000000, 0.000000000000000000 ) ) ;
#190 = EDGE_CURVE ( 'NONE', #6276, #982, #5318, .T. ) ;
#191 = AXIS2_PLACEMENT_3D ( 'NONE', #4745, #5352, #4181 ) ;
#192 = CIRCLE ( 'NONE', #5707, 5.000000000000000000 ) ;
#193 = EDGE_LOOP ( 'NONE', ( #6040, #1662, #7334, #6925 ) ) ;
#194 = CARTESIAN_POINT ( 'NONE',  ( 400.0000000000000000, -12.50000000000000000, -12.95183384698871798 ) ) ;
#195 = EDGE_LOOP ( 'NONE', ( #3741, #7499, #1010, #3595 ) ) ;
#196 = AXIS2_PLACEMENT_3D ( 'NONE', #5443, #2356, #6569 ) ;
#197 = ORIENTED_EDGE ( 'NONE', *, *, #6177, .T. ) ;
#198 = CARTESIAN_POINT ( 'NONE',  ( -1.301042606982605321E-15, -37.50000000000000000, 12.50000000000000000 ) ) ;
#199 = CARTESIAN_POINT ( 'NONE',  ( 13.21904415029483459, 19.40417101989674009, 0.000000000000000000 ) ) ;
#200 = DIRECTION ( 'NONE',  ( -0.000000000000000000, -0.000000000000000000, -1.000000000000000000 ) ) ;
#201 = ORIENTED_EDGE ( 'NONE', *, *, #2548, .F. ) ;
#202 = CYLINDRICAL_SURFACE ( 'NONE', #7486, 24.99999996734561236 ) ;
#203 = ADVANCED_FACE ( 'NONE', ( #4230 ), #7485, .T. ) ;
#204 = CIRCLE ( 'NONE', #6347, 5.000000000000004441 ) ;
#205 = PRODUCT_DEFINITION_SHAPE ( 'NONE', 'NONE',  #7468 ) ;
#206 = CARTESIAN_POINT ( 'NONE',  ( 12.50000000000000000, 0.000000000000000000, 2.500000000000085265 ) ) ;
#207 = DIRECTION ( 'NONE',  ( 0.000000000000000000, -0.000000000000000000, -1.000000000000000000 ) ) ;
#209 = CARTESIAN_POINT ( 'NONE',  ( 0.000000000000000000, 0.000000000000000000, 7.500000000000000000 ) ) ;
#208 = CIRCLE ( 'NONE', #1871, 12.50000000000001066 ) ;
#210 = DIRECTION ( 'NONE',  ( 0.000000000000000000, 0.000000000000000000, 1.000000000000000000 ) ) ;
#211 = ORIENTED_EDGE ( 'NONE', *, *, #2498, .T. ) ;
#212 = CIRCLE ( 'NONE', #5597, 24.99999998367932719 ) ;
#213 = DIRECTION ( 'NONE',  ( 0.000000000000000000, 0.000000000000000000, 1.000000000000000000 ) ) ;
#214 = DIRECTION ( 'NONE',  ( -4.789677997472869028E-16, -1.000000000000000000, 3.541209203328418185E-29 ) ) ;
#215 = ORIENTED_EDGE ( 'NONE', *, *, #2036, .F. ) ;
#216 = PLANE ( 'NONE',  #478 ) ;
#217 = CARTESIAN_POINT ( 'NONE',  ( -36.78095584970496645, -62.29455879088143888, 12.50000000000000000 ) ) ;
#218 = DIRECTION ( 'NONE',  ( 1.387778780781445676E-15, 1.000000000000000000, -0.000000000000000000 ) ) ;
#219 = ADVANCED_FACE ( 'NONE', ( #7176 ), #3001, .F. ) ;
#220 = DIRECTION ( 'NONE',  ( -1.000000000000000000, 0.000000000000000000, 0.000000000000000000 ) ) ;
#221 = VERTEX_POINT ( 'NONE', #3041 ) ;
#222 = AXIS2_PLACEMENT_3D ( 'NONE', #38, #3852, #5502 ) ;
#223 = ADVANCED_FACE ( 'NONE', ( #5439 ), #6682, .T. ) ;
#224 = ORIENTED_EDGE ( 'NONE', *, *, #1037, .F. ) ;
#225 = ADVANCED_FACE ( 'NONE', ( #476, #7811 ), #2320, .T. ) ;
#226 = AXIS2_PLACEMENT_3D ( 'NONE', #4931, #4325, #6784 ) ;
#227 = DIRECTION ( 'NONE',  ( 1.000000000000000000, 0.000000000000000000, 0.000000000000000000 ) ) ;
#228 = ORIENTED_EDGE ( 'NONE', *, *, #5969, .F. ) ;
#229 = CARTESIAN_POINT ( 'NONE',  ( 286.6025403784439050, 75.00000000000002842, 12.50000000000000000 ) ) ;
#230 = EDGE_LOOP ( 'NONE', ( #5895, #6013 ) ) ;
#231 = EDGE_CURVE ( 'NONE', #6488, #3881, #4145, .T. ) ;
#232 = CARTESIAN_POINT ( 'NONE',  ( 296.6025403784437913, 82.50000000000004263, 155.0000000000000000 ) ) ;
#233 = CARTESIAN_POINT ( 'NONE',  ( -0.000000000000000000, 262.5000000000000568, 0.000000000000000000 ) ) ;
#234 = CIRCLE ( 'NONE', #5486, 5.000000000000000888 ) ;
#235 = CIRCLE ( 'NONE', #1138, 12.50000000000000000 ) ;
#236 = EDGE_CURVE ( 'NONE', #6254, #1115, #1341, .T. ) ;
#237 = EDGE_CURVE ( 'NONE', #1544, #2876, #4653, .T. ) ;
#238 = EDGE_LOOP ( 'NONE', ( #6646, #5724, #7322, #559, #4232 ) ) ;
#239 = DIRECTION ( 'NONE',  ( 0.7071067811865517916, 8.659560562354879857E-17, 0.7071067811865431318 ) ) ;
#240 = ORIENTED_EDGE ( 'NONE', *, *, #6695, .T. ) ;
#241 = AXIS2_PLACEMENT_3D ( 'NONE', #5077, #7569, #7530 ) ;
#242 = AXIS2_PLACEMENT_3D ( 'NONE', #2614, #7029, #6306 ) ;
#243 = VERTEX_POINT ( 'NONE', #7446 ) ;
#244 = APPLICATION_CONTEXT ( 'automotive_design' ) ;
#245 = CARTESIAN_POINT ( 'NONE',  ( 412.5000000000001137, 1.530808498934191916E-15, 25.00000000000000000 ) ) ;
#246 = CARTESIAN_POINT ( 'NONE',  ( 0.000000000000000000, 0.000000000000000000, 47.50000000000000000 ) ) ;
#247 = ORIENTED_EDGE ( 'NONE', *, *, #2358, .F. ) ;
#248 = DIRECTION ( 'NONE',  ( 0.000000000000000000, 0.000000000000000000, -1.000000000000000000 ) ) ;
#249 = CIRCLE ( 'NONE', #2019, 12.50000000000000355 ) ;
#250 = ORIENTED_EDGE ( 'NONE', *, *, #6570, .T. ) ;
#251 = EDGE_CURVE ( 'NONE', #1936, #5801, #2874, .T. ) ;
#252 = ITEM_DEFINED_TRANSFORMATION ( 'NONE', 'NONE', #16,  #5785 ) ;
#253 = DIRECTION ( 'NONE',  ( 1.000000000000000000, -0.000000000000000000, -0.000000000000000000 ) ) ;
#254 = DIRECTION ( 'NONE',  ( -0.000000000000000000, -0.000000000000000000, -1.000000000000000000 ) ) ;
#255 = DIRECTION ( 'NONE',  ( 0.000000000000000000, 1.000000000000000000, 0.000000000000000000 ) ) ;
#256 = DIRECTION ( 'NONE',  ( 0.000000000000000000, 0.000000000000000000, -1.000000000000000000 ) ) ;
#257 = ORIENTED_EDGE ( 'NONE', *, *, #7059, .T. ) ;
#258 = DIRECTION ( 'NONE',  ( 0.000000000000000000, 0.000000000000000000, 1.000000000000000000 ) ) ;
#259 = SHAPE_REPRESENTATION_RELATIONSHIP ( 'NONE' , 'NONE' ,  #6910, #2683 ) ;
#260 = VERTEX_POINT ( 'NONE', #6838 ) ;
#261 = DIRECTION ( 'NONE',  ( 0.000000000000000000, 0.000000000000000000, 1.000000000000000000 ) ) ;
#262 = CARTESIAN_POINT ( 'NONE',  ( -32.49999999999997158, 1.387778780781446307E-14, 0.000000000000000000 ) ) ;
#263 = CARTESIAN_POINT ( 'NONE',  ( 412.5000000000000568, 82.50000000000004263, 20.00000000000000000 ) ) ;
#264 = CARTESIAN_POINT ( 'NONE',  ( -37.49999999999993605, 79.24999999999992895, 130.0000000000000000 ) ) ;
#265 = ORIENTED_EDGE ( 'NONE', *, *, #760, .F. ) ;
#266 = ORIENTED_EDGE ( 'NONE', *, *, #7571, .T. ) ;
#267 = CARTESIAN_POINT ( 'NONE',  ( -15.00000000000000000, 2.143131898507867854E-15, 52.50000000000000000 ) ) ;
#268 = VERTEX_POINT ( 'NONE', #6764 ) ;
#269 = FACE_OUTER_BOUND ( 'NONE', #2507, .T. ) ;
#270 = DIRECTION ( 'NONE',  ( -1.000000000000000000, -0.000000000000000000, -0.000000000000000000 ) ) ;
#271 = CARTESIAN_POINT ( 'NONE',  ( 6.495190528383288253, -16.24999999999999645, 7.500000000000000000 ) ) ;
#272 = DIRECTION ( 'NONE',  ( 1.000000000000000000, -1.232595164407830946E-32, -1.710569414459005214E-48 ) ) ;
#273 = EDGE_CURVE ( 'NONE', #7797, #819, #1208, .T. ) ;
#274 = ADVANCED_FACE ( 'NONE', ( #3795 ), #3515, .T. ) ;
#275 = PRODUCT_DEFINITION_SHAPE ( 'NONE', 'NONE',  #6885 ) ;
#276 = EDGE_CURVE ( 'NONE', #5902, #5001, #2575, .T. ) ;
#277 = ORIENTED_EDGE ( 'NONE', *, *, #1080, .F. ) ;
#278 = LINE ( 'NONE', #2723, #2423 ) ;
#279 = VERTEX_POINT ( 'NONE', #3196 ) ;
#280 = EDGE_LOOP ( 'NONE', ( #6094, #597, #2552, #1101 ) ) ;
#281 = DIRECTION ( 'NONE',  ( -1.000000000000000000, -0.000000000000000000, -0.000000000000000000 ) ) ;
#282 = DIRECTION ( 'NONE',  ( 0.000000000000000000, 0.000000000000000000, 1.000000000000000000 ) ) ;
#283 = CARTESIAN_POINT ( 'NONE',  ( 314.1025403784437913, 142.5000000000000000, 125.0000000000000000 ) ) ;
#284 = DIRECTION ( 'NONE',  ( 0.7070068166729618353, 0.7072067315700302226, 0.000000000000000000 ) ) ;
#285 = ORIENTED_EDGE ( 'NONE', *, *, #1155, .T. ) ;
#286 = DIRECTION ( 'NONE',  ( 1.000000000000000000, 0.000000000000000000, 0.000000000000000000 ) ) ;
#287 = DIRECTION ( 'NONE',  ( 1.261617073437677999E-16, -1.000000000000000000, 0.000000000000000000 ) ) ;
#288 = CYLINDRICAL_SURFACE ( 'NONE', #5824, 12.50000000000000000 ) ;
#289 = DIRECTION ( 'NONE',  ( 0.000000000000000000, 0.000000000000000000, -1.000000000000000000 ) ) ;
#290 = CARTESIAN_POINT ( 'NONE',  ( 375.0000000000000000, 15.61249499599599488, -12.50000000000000000 ) ) ;
#291 = EDGE_CURVE ( 'NONE', #4944, #155, #1584, .T. ) ;
#292 = ORIENTED_EDGE ( 'NONE', *, *, #6653, .F. ) ;
#293 = LINE ( 'NONE', #3268, #3948 ) ;
#294 = CARTESIAN_POINT ( 'NONE',  ( 37.50000000000000711, 182.5000000000000000, 12.50000000000000000 ) ) ;
#295 = FILL_AREA_STYLE_COLOUR ( '', #1590 ) ;
#296 = ORIENTED_EDGE ( 'NONE', *, *, #1888, .F. ) ;
#297 = CIRCLE ( 'NONE', #1708, 5.000000000000000000 ) ;
#298 = ORIENTED_EDGE ( 'NONE', *, *, #6249, .T. ) ;
#299 = DIRECTION ( 'NONE',  ( -1.000000000000000000, 0.000000000000000000, 0.000000000000000000 ) ) ;
#300 = ORIENTED_EDGE ( 'NONE', *, *, #5315, .T. ) ;
#301 = DIRECTION ( 'NONE',  ( -0.000000000000000000, -0.000000000000000000, -1.000000000000000000 ) ) ;
#302 = CARTESIAN_POINT ( 'NONE',  ( 42.50000000000000000, 47.50000000000003553, 12.65877081724072362 ) ) ;
#303 = ADVANCED_FACE ( 'NONE', ( #1229 ), #2587, .T. ) ;
#304 = DIRECTION ( 'NONE',  ( 1.000000000000000000, 0.000000000000000000, 0.000000000000000000 ) ) ;
#305 = CARTESIAN_POINT ( 'NONE',  ( 17.50000000000000355, 2.143131898507868643E-15, 82.49999999999998579 ) ) ;
#306 = AXIS2_PLACEMENT_3D ( 'NONE', #1196, #5333, #4802 ) ;
#307 = AXIS2_PLACEMENT_3D ( 'NONE', #6399, #898, #7680 ) ;
#308 = VERTEX_POINT ( 'NONE', #56 ) ;
#309 = DIRECTION ( 'NONE',  ( -0.000000000000000000, 0.000000000000000000, 1.000000000000000000 ) ) ;
#310 = ORIENTED_EDGE ( 'NONE', *, *, #7912, .F. ) ;
#311 = EDGE_CURVE ( 'NONE', #1117, #1102, #5025, .T. ) ;
#312 = CARTESIAN_POINT ( 'NONE',  ( 400.0000000000000568, -25.00000000000000000, 0.000000000000000000 ) ) ;
#313 = EDGE_LOOP ( 'NONE', ( #5764, #1754 ) ) ;
#314 = CYLINDRICAL_SURFACE ( 'NONE', #6244, 12.50000000000000000 ) ;
#315 = CARTESIAN_POINT ( 'NONE',  ( 339.1025403784438481, 150.0000000000000568, 125.0000000000000000 ) ) ;
#316 = AXIS2_PLACEMENT_3D ( 'NONE', #6610, #992, #3446 ) ;
#317 = ADVANCED_FACE ( 'NONE', ( #7480 ), #100, .T. ) ;
#318 = AXIS2_PLACEMENT_3D ( 'NONE', #1100, #546, #3630 ) ;
#319 = AXIS2_PLACEMENT_3D ( 'NONE', #4648, #1727, #4057 ) ;
#320 = PLANE ( 'NONE',  #7361 ) ;
#321 = ADVANCED_FACE ( 'NONE', ( #1380 ), #689, .T. ) ;
#322 = VERTEX_POINT ( 'NONE', #2469 ) ;
#323 = EDGE_CURVE ( 'NONE', #1563, #1167, #4526, .T. ) ;
#324 = CARTESIAN_POINT ( 'NONE',  ( 0.000000000000000000, 47.50000000000003553, 12.50000000000000000 ) ) ;
#325 = LINE ( 'NONE', #7664, #747 ) ;
#326 = DIRECTION ( 'NONE',  ( -0.000000000000000000, -0.000000000000000000, -1.000000000000000000 ) ) ;
#327 = FACE_OUTER_BOUND ( 'NONE', #5998, .T. ) ;
#328 = CIRCLE ( 'NONE', #4299, 12.50000000000000000 ) ;
#329 = CARTESIAN_POINT ( 'NONE',  ( 383.2533226507719633, 17.65289753843946841, 9.421765557058566998 ) ) ;
#330 = ADVANCED_FACE ( 'NONE', ( #6803 ), #6719, .T. ) ;
#331 = FACE_OUTER_BOUND ( 'NONE', #5233, .T. ) ;
#332 = COLOUR_RGB ( '',0.7921568627450980005, 0.8196078431372548767, 0.9333333333333333481 ) ;
#333 = DIRECTION ( 'NONE',  ( 0.000000000000000000, 0.000000000000000000, 1.000000000000000000 ) ) ;
#334 = VERTEX_POINT ( 'NONE', #6163 ) ;
#335 =( NAMED_UNIT ( * ) PLANE_ANGLE_UNIT ( ) SI_UNIT ( $, .RADIAN. ) );
#336 = DIRECTION ( 'NONE',  ( 4.270088556250607616E-16, 1.000000000000000000, -0.000000000000000000 ) ) ;
#337 = CARTESIAN_POINT ( 'NONE',  ( -37.50000000000000000, 4.857225732735047243E-14, 12.50000000000000000 ) ) ;
#338 = DIRECTION ( 'NONE',  ( 1.000000000000000000, 0.000000000000000000, 0.000000000000000000 ) ) ;
#339 = EDGE_LOOP ( 'NONE', ( #7598, #1721, #7213, #3654 ) ) ;
#340 = MECHANICAL_DESIGN_GEOMETRIC_PRESENTATION_REPRESENTATION (  '', ( #3420 ), #6113 ) ;
#341 = SHAPE_REPRESENTATION ( 'Bolt2', ( #5785 ), #4108 ) ;
#342 = VERTEX_POINT ( 'NONE', #2510 ) ;
#343 = ORIENTED_EDGE ( 'NONE', *, *, #7059, .F. ) ;
#344 = CARTESIAN_POINT ( 'NONE',  ( 0.7190441502950423169, -5.595828947448873159, 12.50000000000000000 ) ) ;
#345 = VERTEX_POINT ( 'NONE', #4949 ) ;
#346 = EDGE_CURVE ( 'NONE', #5142, #6431, #1306, .T. ) ;
#347 = CARTESIAN_POINT ( 'NONE',  ( 47.50000000000000711, 0.000000000000000000, 5.000000000000000000 ) ) ;
#348 = AXIS2_PLACEMENT_3D ( 'NONE', #7549, #7663, #286 ) ;
#349 = DIRECTION ( 'NONE',  ( 0.000000000000000000, 0.000000000000000000, 1.000000000000000000 ) ) ;
#350 = FACE_OUTER_BOUND ( 'NONE', #6015, .T. ) ;
#351 = DIRECTION ( 'NONE',  ( -0.000000000000000000, -0.000000000000000000, -1.000000000000000000 ) ) ;
#352 = AXIS2_PLACEMENT_3D ( 'NONE', #7309, #4972, #1287 ) ;
#353 = ORIENTED_EDGE ( 'NONE', *, *, #4920, .T. ) ;
#354 = CYLINDRICAL_SURFACE ( 'NONE', #5629, 37.50000000000000711 ) ;
#355 = ORIENTED_EDGE ( 'NONE', *, *, #2109, .F. ) ;
#356 = CYLINDRICAL_SURFACE ( 'NONE', #4418, 29.99999999999997158 ) ;
#357 = EDGE_LOOP ( 'NONE', ( #1319, #5356 ) ) ;
#358 = CARTESIAN_POINT ( 'NONE',  ( -37.49999999999989342, 187.4999999999999432, 0.000000000000000000 ) ) ;
#359 = VECTOR ( 'NONE', #798, 999.9999999999998863 ) ;
#360 = LINE ( 'NONE', #1436, #2229 ) ;
#361 = CARTESIAN_POINT ( 'NONE',  ( 200.0000000000000000, 0.000000000000000000, 0.000000000000000000 ) ) ;
#362 = CIRCLE ( 'NONE', #1515, 5.000000000000004441 ) ;
#363 = CARTESIAN_POINT ( 'NONE',  ( 296.6025403784439050, 149.9999999999999716, 125.0000000000000000 ) ) ;
#364 = EDGE_CURVE ( 'NONE', #1519, #5920, #5601, .T. ) ;
#365 = VECTOR ( 'NONE', #813, 1000.000000000000000 ) ;
#366 = AXIS2_PLACEMENT_3D ( 'NONE', #6709, #5470, #691 ) ;
#367 = EDGE_LOOP ( 'NONE', ( #1357, #4396, #4864, #3521 ) ) ;
#368 = LINE ( 'NONE', #970, #2555 ) ;
#369 = DIRECTION ( 'NONE',  ( 0.000000000000000000, 0.000000000000000000, 1.000000000000000000 ) ) ;
#370 = CYLINDRICAL_SURFACE ( 'NONE', #7353, 4.999999999999997335 ) ;
#371 = AXIS2_PLACEMENT_3D ( 'NONE', #6748, #1998, #156 ) ;
#372 = AXIS2_PLACEMENT_3D ( 'NONE', #5985, #498, #7152 ) ;
#373 = CARTESIAN_POINT ( 'NONE',  ( 386.8096635605198230, 19.57571528166833019, 4.117265725333339788 ) ) ;
#374 = EDGE_CURVE ( 'NONE', #3850, #1583, #817, .T. ) ;
#375 = ADVANCED_FACE ( 'NONE', ( #7042 ), #7595, .T. ) ;
#376 = DIRECTION ( 'NONE',  ( 0.000000000000000000, 0.000000000000000000, -1.000000000000000000 ) ) ;
#377 = VECTOR ( 'NONE', #7137, 1000.000000000000000 ) ;
#378 = DIRECTION ( 'NONE',  ( 4.789593822244094799E-16, 1.000000000000000000, 5.328524654824031087E-22 ) ) ;
#379 = ORIENTED_EDGE ( 'NONE', *, *, #4066, .F. ) ;
#380 = CARTESIAN_POINT ( 'NONE',  ( 0.000000000000000000, 47.50000000000009237, 130.0000000000000000 ) ) ;
#381 = DIRECTION ( 'NONE',  ( 0.000000000000000000, -0.000000000000000000, -1.000000000000000000 ) ) ;
#382 = DIRECTION ( 'NONE',  ( 0.000000000000000000, 0.000000000000000000, -1.000000000000000000 ) ) ;
#383 = CARTESIAN_POINT ( 'NONE',  ( 0.000000000000000000, 0.000000000000000000, 12.50000000000000000 ) ) ;
#384 = ORIENTED_EDGE ( 'NONE', *, *, #5627, .T. ) ;
#385 = EDGE_CURVE ( 'NONE', #1194, #1704, #2747, .T. ) ;
#386 = UNCERTAINTY_MEASURE_WITH_UNIT (LENGTH_MEASURE( 1.000000000000000082E-05 ), #2222, 'distance_accuracy_value', 'NONE');
#387 = VERTEX_POINT ( 'NONE', #176 ) ;
#388 = B_SPLINE_CURVE_WITH_KNOTS ( 'NONE', 3,
 ( #7794, #5299, #2264, #927, #4425, #2865, #3378, #460, #2907, #5344, #6884, #5829, #329, #2176, #4613, #7071, #1569, #974, #3423, #5867, #373, #7710, #5258, #4652, #9, #2458, #2307, #4173, #7314, #4736, #7196, #2339, #6032, #3068, #7831, #2951, #4892, #4770, #6109, #1730, #3664, #5507, #7232, #5989, #6629, #1692, #1130, #7903, #616, #501, #1812, #538, #3584, #2418 ),
 .UNSPECIFIED., .F., .F.,
 ( 4, 2, 2, 2, 2, 2, 2, 2, 2, 2, 2, 2, 2, 2, 2, 2, 2, 2, 2, 2, 2, 2, 2, 2, 2, 2, 4 ),
 ( 0.04018604478735846031, 0.04269101871805709714, 0.04394350568340633229, 0.04519599264875557437, 0.04644847961410480952, 0.04770096657945405161, 0.05020594051015265374, 0.05145842747550190277, 0.05271091444085115874, 0.05521588837154975393, 0.05646837533689905153, 0.05772086230224834913, 0.05897334926759764673, 0.06022583623294694433, 0.06273081016364553952, 0.06398329712899483712, 0.06523578409434413472, 0.06648827105969341844, 0.06774075802504271604, 0.07024573195574131124, 0.07149821892109066435, 0.07275070588644001746, 0.07525567981713872368, 0.07650816678248806291, 0.07776065374783742989, 0.07901314071318678300, 0.08026562767853613611 ),
 .UNSPECIFIED. ) ;
#389 = VERTEX_POINT ( 'NONE', #5722 ) ;
#390 = ORIENTED_EDGE ( 'NONE', *, *, #7784, .F. ) ;
#391 = DIRECTION ( 'NONE',  ( -1.000000000000000000, 0.000000000000000000, 0.000000000000000000 ) ) ;
#392 = DIRECTION ( 'NONE',  ( 1.000000000000000000, 0.000000000000000000, 0.000000000000000000 ) ) ;
#393 = VERTEX_POINT ( 'NONE', #5107 ) ;
#394 = CARTESIAN_POINT ( 'NONE',  ( 0.000000000000000000, 0.000000000000000000, 92.50000000000000000 ) ) ;
#395 = EDGE_CURVE ( 'NONE', #2843, #1677, #2239, .T. ) ;
#396 = ORIENTED_EDGE ( 'NONE', *, *, #1409, .T. ) ;
#397 = DIRECTION ( 'NONE',  ( -0.000000000000000000, -0.000000000000000000, -1.000000000000000000 ) ) ;
#399 = EDGE_LOOP ( 'NONE', ( #7198, #2677, #721, #3048 ) ) ;
#398 = VECTOR ( 'NONE', #6962, 1000.000000000000114 ) ;
#400 = DIRECTION ( 'NONE',  ( 1.000000000000000000, 0.000000000000000000, 0.000000000000000000 ) ) ;
#401 = EDGE_LOOP ( 'NONE', ( #6678, #4952, #1055, #6847 ) ) ;
#402 = CARTESIAN_POINT ( 'NONE',  ( 200.0000000000000000, 0.000000000000000000, 12.50000000000000000 ) ) ;
#403 = DIRECTION ( 'NONE',  ( 1.000000000000000000, 0.000000000000000000, 0.000000000000000000 ) ) ;
#404 = LINE ( 'NONE', #1042, #2411 ) ;
#405 = DIRECTION ( 'NONE',  ( -0.000000000000000000, -0.000000000000000000, -1.000000000000000000 ) ) ;
#406 = AXIS2_PLACEMENT_3D ( 'NONE', #6275, #333, #5061 ) ;
#407 = ORIENTED_EDGE ( 'NONE', *, *, #6151, .F. ) ;
#408 = ORIENTED_EDGE ( 'NONE', *, *, #2734, .F. ) ;
#409 = PRODUCT_DEFINITION_SHAPE ( 'NONE', 'NONE',  #7906 ) ;
#410 = CIRCLE ( 'NONE', #3617, 11.64999999999996660 ) ;
#411 = FACE_OUTER_BOUND ( 'NONE', #2301, .T. ) ;
#412 = CARTESIAN_POINT ( 'NONE',  ( 38.21904415029484170, 19.40417101989674009, 0.000000000000000000 ) ) ;
#413 = CARTESIAN_POINT ( 'NONE',  ( 412.5000000000000568, 75.00000000000001421, 20.00000000000000000 ) ) ;
#414 = EDGE_CURVE ( 'NONE', #2350, #2221, #5040, .T. ) ;
#415 = DIRECTION ( 'NONE',  ( 1.000000000000000000, -4.625929269271489858E-16, 0.000000000000000000 ) ) ;
#416 = CARTESIAN_POINT ( 'NONE',  ( 12.50000000000002309, 225.0000000000000284, 12.50000000000000000 ) ) ;
#417 = CARTESIAN_POINT ( 'NONE',  ( 13.21904415029483459, 19.40417101989674009, 12.50000000000000000 ) ) ;
#418 = APPLICATION_PROTOCOL_DEFINITION ( 'draft international standard', 'automotive_design', 1998, #5359 ) ;
#419 = ORIENTED_EDGE ( 'NONE', *, *, #1254, .F. ) ;
#420 = EDGE_CURVE ( 'NONE', #3389, #4483, #5139, .T. ) ;
#421 = FACE_OUTER_BOUND ( 'NONE', #3553, .T. ) ;
#422 = CARTESIAN_POINT ( 'NONE',  ( 6.495190528383280260, 11.25000000000000000, 7.500000000000000000 ) ) ;
#423 = FACE_OUTER_BOUND ( 'NONE', #6935, .T. ) ;
#424 = ORIENTED_EDGE ( 'NONE', *, *, #1837, .F. ) ;
#425 = ADVANCED_FACE ( 'NONE', ( #5065 ), #1542, .T. ) ;
#426 = ORIENTED_EDGE ( 'NONE', *, *, #43, .T. ) ;
#427 = ORIENTED_EDGE ( 'NONE', *, *, #1008, .T. ) ;
#428 = CIRCLE ( 'NONE', #166, 37.50000000000003553 ) ;
#429 = ADVANCED_FACE ( 'NONE', ( #5224 ), #4545, .F. ) ;
#430 = SHAPE_REPRESENTATION_RELATIONSHIP ( 'NONE' , 'NONE' ,  #2073, #3260 ) ;
#431 = ORIENTED_EDGE ( 'NONE', *, *, #1211, .F. ) ;
#432 = FACE_OUTER_BOUND ( 'NONE', #1200, .T. ) ;
#433 = DIRECTION ( 'NONE',  ( 1.000000000000000000, -9.251858538542979716E-16, 0.000000000000000000 ) ) ;
#434 = ORIENTED_EDGE ( 'NONE', *, *, #5862, .T. ) ;
#435 = DIRECTION ( 'NONE',  ( 0.000000000000000000, 0.000000000000000000, -1.000000000000000000 ) ) ;
#436 = CARTESIAN_POINT ( 'NONE',  ( 12.99038105676657651, -1.301042606982605321E-15, 7.500000000000000000 ) ) ;
#437 = CIRCLE ( 'NONE', #4903, 35.78244274809159720 ) ;
#438 = ORIENTED_EDGE ( 'NONE', *, *, #1694, .F. ) ;
#439 = LINE ( 'NONE', #1158, #5506 ) ;
#440 = ORIENTED_EDGE ( 'NONE', *, *, #5822, .T. ) ;
#441 = AXIS2_PLACEMENT_3D ( 'NONE', #1979, #6881, #1823 ) ;
#442 = LINE ( 'NONE', #3529, #7380 ) ;
#443 = VERTEX_POINT ( 'NONE', #979 ) ;
#444 = SHAPE_REPRESENTATION ( 'Sheet Metal Base', ( #5785 ), #6420 ) ;
#445 = LINE ( 'NONE', #2814, #3060 ) ;
#446 = DIRECTION ( 'NONE',  ( 0.000000000000000000, 0.000000000000000000, -1.000000000000000000 ) ) ;
#447 = VECTOR ( 'NONE', #405, 1000.000000000000000 ) ;
#448 = AXIS2_PLACEMENT_3D ( 'NONE', #7739, #4869, #4683 ) ;
#449 = VECTOR ( 'NONE', #4259, 1000.000000000000000 ) ;
#450 = ORIENTED_EDGE ( 'NONE', *, *, #864, .F. ) ;
#451 = ORIENTED_EDGE ( 'NONE', *, *, #4286, .T. ) ;
#452 = AXIS2_PLACEMENT_3D ( 'NONE', #4358, #6815, #1317 ) ;
#453 =( GEOMETRIC_REPRESENTATION_CONTEXT ( 3 ) GLOBAL_UNCERTAINTY_ASSIGNED_CONTEXT ( ( #3202 ) ) GLOBAL_UNIT_ASSIGNED_CONTEXT ( ( #1271, #2470, #555 ) ) REPRESENTATION_CONTEXT ( 'NONE', 'WORKASPACE' ) );
#454 = CIRCLE ( 'NONE', #3146, 31.24999999999998579 ) ;
#455 = ADVANCED_FACE ( 'NONE', ( #6999 ), #897, .F. ) ;
#456 = CARTESIAN_POINT ( 'NONE',  ( -12.50000000000000000, 0.000000000000000000, 12.50000000000000000 ) ) ;
#457 = CARTESIAN_POINT ( 'NONE',  ( 25.71904415029483459, 19.40417101989674009, 12.50000000000000000 ) ) ;
#458 = DIRECTION ( 'NONE',  ( 1.000000000000000000, 0.000000000000000000, -0.000000000000000000 ) ) ;
#459 = CARTESIAN_POINT ( 'NONE',  ( 15.64999999999999680, 1.916572240665607593E-15, 195.9999999999999716 ) ) ;
#460 = CARTESIAN_POINT ( 'NONE',  ( 380.2287650028787880, 16.46093790404528789, 11.36110438390628197 ) ) ;
#461 = AXIS2_PLACEMENT_3D ( 'NONE', #436, #4234, #5280 ) ;
#462 = CARTESIAN_POINT ( 'NONE',  ( 400.0000000000000000, 12.50000000000000000, 12.95183384698871620 ) ) ;
#463 = DIRECTION ( 'NONE',  ( -4.789152899817859511E-16, -0.9999999999999997780, 4.157528252970400373E-20 ) ) ;
#464 = ORIENTED_EDGE ( 'NONE', *, *, #7246, .F. ) ;
#465 = DIRECTION ( 'NONE',  ( 0.000000000000000000, 0.000000000000000000, 1.000000000000000000 ) ) ;
#467 = FACE_BOUND ( 'NONE', #5993, .T. ) ;
#466 = VECTOR ( 'NONE', #1352, 1000.000000000000000 ) ;
#468 = PLANE ( 'NONE',  #1082 ) ;
#469 = ORIENTED_EDGE ( 'NONE', *, *, #2265, .T. ) ;
#470 = EDGE_CURVE ( 'NONE', #4246, #3773, #2141, .T. ) ;
#471 = CIRCLE ( 'NONE', #4940, 12.50000000000001066 ) ;
#472 = ORIENTED_EDGE ( 'NONE', *, *, #6692, .T. ) ;
#473 = EDGE_CURVE ( 'NONE', #116, #3864, #3982, .T. ) ;
#474 = ORIENTED_EDGE ( 'NONE', *, *, #7618, .F. ) ;
#475 =( NAMED_UNIT ( * ) PLANE_ANGLE_UNIT ( ) SI_UNIT ( $, .RADIAN. ) );
#476 = FACE_OUTER_BOUND ( 'NONE', #5695, .T. ) ;
#477 = VERTEX_POINT ( 'NONE', #934 ) ;
#478 = AXIS2_PLACEMENT_3D ( 'NONE', #1977, #2666, #97 ) ;
#479 = CARTESIAN_POINT ( 'NONE',  ( -24.28095581706361372, 2.657566677470048251E-15, 0.000000000000000000 ) ) ;
#480 = EDGE_CURVE ( 'NONE', #3444, #2321, #3270, .T. ) ;
#481 = VERTEX_POINT ( 'NONE', #2183 ) ;
#482 = AXIS2_PLACEMENT_3D ( 'NONE', #1216, #6036, #3588 ) ;
#483 = EDGE_CURVE ( 'NONE', #5349, #477, #7076, .T. ) ;
#484 = DIRECTION ( 'NONE',  ( 0.000000000000000000, -0.000000000000000000, -1.000000000000000000 ) ) ;
#485 = ORIENTED_EDGE ( 'NONE', *, *, #7101, .T. ) ;
#486 = DIRECTION ( 'NONE',  ( -0.7071067811865479058, 8.659560562354930393E-17, -0.7071067811865472397 ) ) ;
#487 = ORIENTED_EDGE ( 'NONE', *, *, #4999, .T. ) ;
#488 = DIRECTION ( 'NONE',  ( -0.8660254037844385966, 0.5000000000000003331, 0.000000000000000000 ) ) ;
#489 = CARTESIAN_POINT ( 'NONE',  ( 2.775557561562891351E-14, 225.0000000000000284, 12.50000000000000000 ) ) ;
#490 = EDGE_CURVE ( 'NONE', #6450, #7344, #1575, .T. ) ;
#491 = EDGE_CURVE ( 'NONE', #4246, #1194, #7560, .T. ) ;
#492 = CIRCLE ( 'NONE', #3934, 12.50000000000000000 ) ;
#493 = EDGE_LOOP ( 'NONE', ( #5975, #1539, #5084, #6737 ) ) ;
#494 = ORIENTED_EDGE ( 'NONE', *, *, #6021, .T. ) ;
#495 = AXIS2_PLACEMENT_3D ( 'NONE', #1873, #6693, #562 ) ;
#496 = VECTOR ( 'NONE', #6062, 1000.000000000000000 ) ;
#497 = DIRECTION ( 'NONE',  ( 1.000000000000000000, 0.000000000000000000, 0.000000000000000000 ) ) ;
#498 = DIRECTION ( 'NONE',  ( 0.000000000000000000, -1.000000000000000000, 0.000000000000000000 ) ) ;
#499 = CARTESIAN_POINT ( 'NONE',  ( 0.000000000000000000, 0.000000000000000000, 200.0000000000000000 ) ) ;
#500 = DIRECTION ( 'NONE',  ( -0.000000000000000000, -0.000000000000000000, -1.000000000000000000 ) ) ;
#501 = CARTESIAN_POINT ( 'NONE',  ( 377.1106974111345380, 15.74939801616919866, -12.32751675873151598 ) ) ;
#502 = AXIS2_PLACEMENT_3D ( 'NONE', #7116, #975, #2909 ) ;
#503 = AXIS2_PLACEMENT_3D ( 'NONE', #2813, #5247, #2205 ) ;
#504 = EDGE_CURVE ( 'NONE', #4687, #756, #6958, .T. ) ;
#505 = FACE_BOUND ( 'NONE', #3911, .T. ) ;
#506 = AXIS2_PLACEMENT_3D ( 'NONE', #6371, #2247, #3882 ) ;
#507 = CYLINDRICAL_SURFACE ( 'NONE', #1385, 37.50000000000000711 ) ;
#508 = AXIS2_PLACEMENT_3D ( 'NONE', #3751, #3075, #3787 ) ;
#509 = CARTESIAN_POINT ( 'NONE',  ( -25.00000000000000000, 25.00000000000000000, 0.000000000000000000 ) ) ;
#510 = DIRECTION ( 'NONE',  ( 1.000000000000000000, 0.000000000000000000, 0.000000000000000000 ) ) ;
#511 = VERTEX_POINT ( 'NONE', #263 ) ;
#512 = AXIS2_PLACEMENT_3D ( 'NONE', #3984, #4796, #7779 ) ;
#513 = AXIS2_PLACEMENT_3D ( 'NONE', #5625, #3065, #6 ) ;
#514 = ORIENTED_EDGE ( 'NONE', *, *, #7045, .F. ) ;
#515 = ORIENTED_EDGE ( 'NONE', *, *, #3809, .F. ) ;
#516 = FILL_AREA_STYLE ('',( #6121 ) ) ;
#517 = CARTESIAN_POINT ( 'NONE',  ( 398.0000000000001137, 0.000000000000000000, 0.000000000000000000 ) ) ;
#518 = ORIENTED_EDGE ( 'NONE', *, *, #3537, .T. ) ;
#519 = CYLINDRICAL_SURFACE ( 'NONE', #5579, 12.50000000000000000 ) ;
#520 = EDGE_LOOP ( 'NONE', ( #5499, #7180, #5921, #6159 ) ) ;
#521 = CARTESIAN_POINT ( 'NONE',  ( -10.82531754730547924, 13.75000000000000000, 7.500000000000000000 ) ) ;
#522 = ORIENTED_EDGE ( 'NONE', *, *, #7865, .F. ) ;
#523 = CARTESIAN_POINT ( 'NONE',  ( 372.0751627177024830, -15.87901657654723664, -12.16010032319875833 ) ) ;
#524 = ORIENTED_EDGE ( 'NONE', *, *, #2580, .T. ) ;
#525 = EDGE_CURVE ( 'NONE', #6373, #2940, #4779, .T. ) ;
#526 = CARTESIAN_POINT ( 'NONE',  ( -25.00000000000000000, 0.000000000000000000, 0.000000000000000000 ) ) ;
#527 = CARTESIAN_POINT ( 'NONE',  ( 0.7190441502950353225, 87.70544117646394966, 12.50000000000000000 ) ) ;
#528 = ADVANCED_FACE ( 'NONE', ( #7165 ), #5426, .F. ) ;
#529 = ORIENTED_EDGE ( 'NONE', *, *, #2971, .F. ) ;
#530 = VERTEX_POINT ( 'NONE', #1780 ) ;
#531 = ADVANCED_FACE ( 'NONE', ( #7203 ), #1619, .F. ) ;
#532 = DIRECTION ( 'NONE',  ( 0.000000000000000000, 0.000000000000000000, -1.000000000000000000 ) ) ;
#533 = DIRECTION ( 'NONE',  ( 0.000000000000000000, -1.481552359947913884E-16, 1.000000000000000000 ) ) ;
#534 = DIRECTION ( 'NONE',  ( 0.000000000000000000, 0.000000000000000000, -1.000000000000000000 ) ) ;
#535 = FACE_OUTER_BOUND ( 'NONE', #6691, .T. ) ;
#536 =( GEOMETRIC_REPRESENTATION_CONTEXT ( 3 ) GLOBAL_UNCERTAINTY_ASSIGNED_CONTEXT ( ( #5271 ) ) GLOBAL_UNIT_ASSIGNED_CONTEXT ( ( #94, #7442, #5550 ) ) REPRESENTATION_CONTEXT ( 'NONE', 'WORKASPACE' ) );
#537 = FACE_OUTER_BOUND ( 'NONE', #7292, .T. ) ;
#538 = CARTESIAN_POINT ( 'NONE',  ( 375.8507511021305163, 15.62998136526340076, -12.47825053757332370 ) ) ;
#539 = PRODUCT_DEFINITION_FORMATION_WITH_SPECIFIED_SOURCE ( 'ANY', '', #2574, .NOT_KNOWN. ) ;
#540 = CARTESIAN_POINT ( 'NONE',  ( 25.71904415029483459, -5.595828947448873159, 12.50000000000000000 ) ) ;
#541 = DIRECTION ( 'NONE',  ( -4.789152899817846692E-16, -0.9999999999999998890, 4.157528252997517467E-20 ) ) ;
#542 = DIRECTION ( 'NONE',  ( -1.000000000000000000, 0.000000000000000000, 0.000000000000000000 ) ) ;
#543 = CARTESIAN_POINT ( 'NONE',  ( -12.50000000000000000, 0.000000000000000000, 90.00000000000000000 ) ) ;
#544 = PLANE ( 'NONE',  #945 ) ;
#545 = EDGE_CURVE ( 'NONE', #3577, #4697, #5265, .T. ) ;
#546 = DIRECTION ( 'NONE',  ( -0.000000000000000000, 0.000000000000000000, 1.000000000000000000 ) ) ;
#547 = ORIENTED_EDGE ( 'NONE', *, *, #6445, .T. ) ;
#548 = EDGE_LOOP ( 'NONE', ( #3367, #4727, #4586, #2245 ) ) ;
#549 = APPLICATION_CONTEXT ( 'automotive_design' ) ;
#550 = ORIENTED_EDGE ( 'NONE', *, *, #4306, .F. ) ;
#551 =( NAMED_UNIT ( * ) PLANE_ANGLE_UNIT ( ) SI_UNIT ( $, .RADIAN. ) );
#552 = LINE ( 'NONE', #3634, #2145 ) ;
#553 = CARTESIAN_POINT ( 'NONE',  ( 326.6025403784438481, 150.0000000000000568, 125.0000000000000000 ) ) ;
#554 = ADVANCED_FACE ( 'NONE', ( #1738 ), #3476, .T. ) ;
#555 =( NAMED_UNIT ( * ) SI_UNIT ( $, .STERADIAN. ) SOLID_ANGLE_UNIT ( ) );
#556 = VERTEX_POINT ( 'NONE', #5306 ) ;
#557 = CARTESIAN_POINT ( 'NONE',  ( 375.0000000000000000, -12.50000000000000355, -12.50000000000000000 ) ) ;
#558 = DIRECTION ( 'NONE',  ( -4.789677997474686366E-16, -1.000000000000000000, 0.000000000000000000 ) ) ;
#559 = ORIENTED_EDGE ( 'NONE', *, *, #1062, .T. ) ;
#560 = CARTESIAN_POINT ( 'NONE',  ( 366.4515434226340176, -17.79791451299709948, -9.128686039268288255 ) ) ;
#561 = ORIENTED_EDGE ( 'NONE', *, *, #6531, .F. ) ;
#562 = DIRECTION ( 'NONE',  ( 1.000000000000000000, 0.000000000000000000, 0.000000000000000000 ) ) ;
#563 = DIRECTION ( 'NONE',  ( -0.000000000000000000, -0.000000000000000000, -1.000000000000000000 ) ) ;
#564 = VECTOR ( 'NONE', #4224, 1000.000000000000000 ) ;
#565 = ORIENTED_EDGE ( 'NONE', *, *, #7553, .F. ) ;
#566 = CLOSED_SHELL ( 'NONE', ( #4803, #7833, #4, #588, #5189, #2945, #7825, #1974, #223, #578, #4507, #4448, #7790, #3968, #3765, #3719, #6908, #6228, #5216, #5664, #2044, #4485, #203, #6599 ) ) ;
#567 = EDGE_CURVE ( 'NONE', #3797, #109, #5955, .T. ) ;
#568 = ORIENTED_EDGE ( 'NONE', *, *, #7584, .F. ) ;
#569 = ADVANCED_FACE ( 'NONE', ( #2956, #423 ), #1665, .T. ) ;
#570 = CARTESIAN_POINT ( 'NONE',  ( 382.6319868782507569, -17.37589182433591972, 9.907690019304302709 ) ) ;
#571 = CARTESIAN_POINT ( 'NONE',  ( 296.6025403784437913, 144.9999999999999716, 0.000000000000000000 ) ) ;
#572 = DIRECTION ( 'NONE',  ( 1.000000000000000000, 0.000000000000000000, 0.000000000000000000 ) ) ;
#573 = DIRECTION ( 'NONE',  ( 0.000000000000000000, 0.000000000000000000, 1.000000000000000000 ) ) ;
#574 = VECTOR ( 'NONE', #1209, 1000.000000000000000 ) ;
#575 = AXIS2_PLACEMENT_3D ( 'NONE', #4907, #4309, #1270 ) ;
#576 = DIRECTION ( 'NONE',  ( 0.000000000000000000, -1.000000000000000000, 0.000000000000000000 ) ) ;
#577 = CARTESIAN_POINT ( 'NONE',  ( 286.6025403784437913, 135.0000000000000000, 12.50000000000000000 ) ) ;
#578 = ADVANCED_FACE ( 'NONE', ( #1099 ), #6038, .F. ) ;
#579 = EDGE_CURVE ( 'NONE', #2973, #7220, #2385, .T. ) ;
#580 = VECTOR ( 'NONE', #728, 1000.000000000000000 ) ;
#581 = CIRCLE ( 'NONE', #307, 13.00000000000000178 ) ;
#582 = CARTESIAN_POINT ( 'NONE',  ( -11.64999999999996660, 0.000000000000000000, 200.0000000000000000 ) ) ;
#583 = CARTESIAN_POINT ( 'NONE',  ( 375.0000000000000000, -12.50000000000000355, 3.061616997868383043E-15 ) ) ;
#584 = DIRECTION ( 'NONE',  ( 1.000000000000000000, 0.000000000000000000, 0.000000000000000000 ) ) ;
#585 = CARTESIAN_POINT ( 'NONE',  ( 150.0000000000000000, 1.836970198721029747E-14, 0.000000000000000000 ) ) ;
#586 = VECTOR ( 'NONE', #272, 1000.000000000000000 ) ;
#587 = CIRCLE ( 'NONE', #3639, 12.50000000000001066 ) ;
#588 = ADVANCED_FACE ( 'NONE', ( #7121 ), #4700, .F. ) ;
#589 = EDGE_LOOP ( 'NONE', ( #4960, #6697, #7720, #5853 ) ) ;
#590 =( LENGTH_UNIT ( ) NAMED_UNIT ( * ) SI_UNIT ( .MILLI., .METRE. ) );
#591 = ORIENTED_EDGE ( 'NONE', *, *, #3316, .T. ) ;
#592 = FACE_OUTER_BOUND ( 'NONE', #7147, .T. ) ;
#593 = DIRECTION ( 'NONE',  ( -4.789677997474686366E-16, -1.000000000000000000, -0.000000000000000000 ) ) ;
#594 = ORIENTED_EDGE ( 'NONE', *, *, #4286, .F. ) ;
#595 = CYLINDRICAL_SURFACE ( 'NONE', #3402, 15.64999999999999680 ) ;
#596 = CIRCLE ( 'NONE', #2906, 25.00000000000000000 ) ;
#597 = ORIENTED_EDGE ( 'NONE', *, *, #4395, .T. ) ;
#598 = ADVANCED_FACE ( 'NONE', ( #4659 ), #544, .T. ) ;
#599 = DIRECTION ( 'NONE',  ( 1.000000000000000000, 0.000000000000000000, 0.000000000000000000 ) ) ;
#600 = VERTEX_POINT ( 'NONE', #2272 ) ;
#601 = CARTESIAN_POINT ( 'NONE',  ( 63.21904415029505486, 62.70544120911855401, 0.000000000000000000 ) ) ;
#602 = VECTOR ( 'NONE', #5887, 1000.000000000000000 ) ;
#603 = VERTEX_POINT ( 'NONE', #1057 ) ;
#604 = SURFACE_STYLE_USAGE ( .BOTH. , #4961 ) ;
#605 = DIRECTION ( 'NONE',  ( 0.000000000000000000, 0.000000000000000000, -1.000000000000000000 ) ) ;
#606 = MECHANICAL_DESIGN_GEOMETRIC_PRESENTATION_REPRESENTATION (  '', ( #4056 ), #729 ) ;
#607 = ORIENTED_EDGE ( 'NONE', *, *, #3175, .F. ) ;
#608 = ORIENTED_EDGE ( 'NONE', *, *, #3986, .F. ) ;
#609 = ORIENTED_EDGE ( 'NONE', *, *, #5693, .F. ) ;
#610 = CARTESIAN_POINT ( 'NONE',  ( 382.3090924919189888, -17.23604965026853009, 10.14822696828370319 ) ) ;
#611 = CARTESIAN_POINT ( 'NONE',  ( 387.4113400591389222, -19.94427247194493802, -1.702902647306309358 ) ) ;
#612 = CARTESIAN_POINT ( 'NONE',  ( 10.82531754730548279, -13.74999999999999645, 0.000000000000000000 ) ) ;
#614 = CARTESIAN_POINT ( 'NONE',  ( 190.0000000000000000, 12.50000000000000000, 21.65063509461096913 ) ) ;
#613 = VECTOR ( 'NONE', #5624, 1000.000000000000000 ) ;
#615 = CARTESIAN_POINT ( 'NONE',  ( 286.6025403784437913, 135.0000000000000000, 12.50000000000000000 ) ) ;
#616 = CARTESIAN_POINT ( 'NONE',  ( 377.9248372822975170, 15.87901657654723664, -12.16010032319875833 ) ) ;
#617 = VECTOR ( 'NONE', #6785, 1000.000000000000000 ) ;
#618 = LINE ( 'NONE', #6112, #1900 ) ;
#619 = CARTESIAN_POINT ( 'NONE',  ( -25.00000000000000000, -25.00000000000000000, 0.000000000000000000 ) ) ;
#620 = LINE ( 'NONE', #6874, #4152 ) ;
#621 = LINE ( 'NONE', #2464, #6448 ) ;
#622 = AXIS2_PLACEMENT_3D ( 'NONE', #1717, #4162, #1598 ) ;
#623 = ADVANCED_FACE ( 'NONE', ( #7279, #3510, #467 ), #2915, .T. ) ;
#624 = VECTOR ( 'NONE', #6475, 1000.000000000000000 ) ;
#625 = ADVANCED_FACE ( 'NONE', ( #1700 ), #4140, .F. ) ;
#626 = ORIENTED_EDGE ( 'NONE', *, *, #4262, .T. ) ;
#627 = AXIS2_PLACEMENT_3D ( 'NONE', #1428, #3879, #6326 ) ;
#628 = CIRCLE ( 'NONE', #3315, 12.50000000000000355 ) ;
#629 = ORIENTED_EDGE ( 'NONE', *, *, #810, .F. ) ;
#630 = LINE ( 'NONE', #7288, #2124 ) ;
#631 = CARTESIAN_POINT ( 'NONE',  ( 0.000000000000000000, -37.50000000000000000, 12.50000000000000000 ) ) ;
#632 = CARTESIAN_POINT ( 'NONE',  ( -6.495190528383287365, 11.25000000000000000, 7.500000000000000000 ) ) ;
#633 = ADVANCED_FACE ( 'NONE', ( #48 ), #1218, .T. ) ;
#634 = DIRECTION ( 'NONE',  ( -0.000000000000000000, 0.000000000000000000, 1.000000000000000000 ) ) ;
#635 = ORIENTED_EDGE ( 'NONE', *, *, #3722, .F. ) ;
#636 = DIRECTION ( 'NONE',  ( -1.000000000000000000, 0.000000000000000000, 0.000000000000000000 ) ) ;
#637 = CIRCLE ( 'NONE', #1657, 37.50000000000003553 ) ;
#638 = UNCERTAINTY_MEASURE_WITH_UNIT (LENGTH_MEASURE( 1.000000000000000082E-05 ), #3084, 'distance_accuracy_value', 'NONE');
#639 = CARTESIAN_POINT ( 'NONE',  ( 371.6813660871608818, 15.95663992257128427, 12.05857923940197907 ) ) ;
#640 = ORIENTED_EDGE ( 'NONE', *, *, #2125, .F. ) ;
#641 = LINE ( 'NONE', #3735, #5060 ) ;
#642 = VERTEX_POINT ( 'NONE', #4372 ) ;
#643 = DIRECTION ( 'NONE',  ( -1.000000000000000000, -0.000000000000000000, -0.000000000000000000 ) ) ;
#644 = ADVANCED_FACE ( 'NONE', ( #4987 ), #6792, .T. ) ;
#645 = ORIENTED_EDGE ( 'NONE', *, *, #5923, .T. ) ;
#646 = VERTEX_POINT ( 'NONE', #7437 ) ;
#647 = EDGE_LOOP ( 'NONE', ( #2566, #3992, #6282, #4635, #3699, #5556, #5162, #7459 ) ) ;
#648 = FACE_OUTER_BOUND ( 'NONE', #1364, .T. ) ;
#649 = LINE ( 'NONE', #3103, #1509 ) ;
#650 = DIRECTION ( 'NONE',  ( 1.000000000000000000, 0.000000000000000000, 0.000000000000000000 ) ) ;
#651 = CARTESIAN_POINT ( 'NONE',  ( 199.9999999999998863, 225.0000000000000284, 0.000000000000000000 ) ) ;
#652 = CARTESIAN_POINT ( 'NONE',  ( 0.7190441502950353225, 62.70544120911855401, 0.000000000000000000 ) ) ;
#653 =( REPRESENTATION_RELATIONSHIP ('NONE','NONE', #6292, #7467 ) REPRESENTATION_RELATIONSHIP_WITH_TRANSFORMATION ( #3859 )SHAPE_REPRESENTATION_RELATIONSHIP( ) );
#654 = DIRECTION ( 'NONE',  ( 1.000000000000000000, 0.000000000000000000, 0.000000000000000000 ) ) ;
#655 = LINE ( 'NONE', #7469, #7008 ) ;
#656 = FACE_OUTER_BOUND ( 'NONE', #7185, .T. ) ;
#657 = DIRECTION ( 'NONE',  ( -1.295260195396012940E-15, 1.000000000000000000, 0.000000000000000000 ) ) ;
#658 = DIRECTION ( 'NONE',  ( 0.000000000000000000, -0.000000000000000000, 1.000000000000000000 ) ) ;
#659 = AXIS2_PLACEMENT_3D ( 'NONE', #4017, #1571, #7073 ) ;
#660 = ORIENTED_EDGE ( 'NONE', *, *, #491, .T. ) ;
#661 = EDGE_CURVE ( 'NONE', #1300, #698, #6721, .T. ) ;
#662 = ORIENTED_EDGE ( 'NONE', *, *, #6661, .F. ) ;
#663 = SURFACE_STYLE_FILL_AREA ( #7516 ) ;
#664 = DIRECTION ( 'NONE',  ( -0.000000000000000000, 0.000000000000000000, 1.000000000000000000 ) ) ;
#665 = DIRECTION ( 'NONE',  ( 1.000000000000000000, 0.000000000000000000, 0.000000000000000000 ) ) ;
#666 = EDGE_CURVE ( 'NONE', #5450, #5144, #3150, .T. ) ;
#667 = ORIENTED_EDGE ( 'NONE', *, *, #3236, .T. ) ;
#668 = LINE ( 'NONE', #1189, #7500 ) ;
#669 = EDGE_CURVE ( 'NONE', #7782, #6179, #2463, .T. ) ;
#670 = ORIENTED_EDGE ( 'NONE', *, *, #5066, .T. ) ;
#671 = DIRECTION ( 'NONE',  ( -0.000000000000000000, -0.000000000000000000, -1.000000000000000000 ) ) ;
#672 = ORIENTED_EDGE ( 'NONE', *, *, #2727, .T. ) ;
#673 = FACE_OUTER_BOUND ( 'NONE', #4002, .T. ) ;
#674 = ORIENTED_EDGE ( 'NONE', *, *, #4625, .T. ) ;
#675 = FACE_BOUND ( 'NONE', #4183, .T. ) ;
#676 = ADVANCED_BREP_SHAPE_REPRESENTATION ( '', ( #4034, #5785 ), #3097 ) ;
#677 = FACE_OUTER_BOUND ( 'NONE', #1313, .T. ) ;
#678 = EDGE_LOOP ( 'NONE', ( #1523, #3489, #674, #1591 ) ) ;
#679 = EDGE_LOOP ( 'NONE', ( #2751, #4665, #1825, #7638, #6357 ) ) ;
#680 = EDGE_LOOP ( 'NONE', ( #1068, #3296 ) ) ;
#681 = CARTESIAN_POINT ( 'NONE',  ( 378.3186339128393456, -15.95663992257128427, 12.05857923940197907 ) ) ;
#682 = CARTESIAN_POINT ( 'NONE',  ( 381.3105327226213035, -16.82862359362766469, -10.81999899256329911 ) ) ;
#683 = LINE ( 'NONE', #1884, #4208 ) ;
#684 = CARTESIAN_POINT ( 'NONE',  ( -32.49999999999990052, 177.4999999999999432, 0.000000000000000000 ) ) ;
#685 = FACE_OUTER_BOUND ( 'NONE', #1976, .T. ) ;
#686 = VECTOR ( 'NONE', #593, 1000.000000000000000 ) ;
#687 = ADVANCED_FACE ( 'NONE', ( #1931, #3034 ), #1818, .T. ) ;
#688 = ITEM_DEFINED_TRANSFORMATION ( 'NONE', 'NONE', #1174,  #5785 ) ;
#689 = CONICAL_SURFACE ( 'NONE', #1714, 31.78244274809162562, 0.7853981633974447263 ) ;
#690 = CARTESIAN_POINT ( 'NONE',  ( 400.0000000000000000, 20.00000000000000000, 0.000000000000000000 ) ) ;
#691 = DIRECTION ( 'NONE',  ( 1.000000000000000000, 0.000000000000000000, 0.000000000000000000 ) ) ;
#692 = DIRECTION ( 'NONE',  ( -0.000000000000000000, -0.000000000000000000, 1.000000000000000000 ) ) ;
#693 = DIRECTION ( 'NONE',  ( -0.000000000000000000, -0.000000000000000000, -1.000000000000000000 ) ) ;
#694 = APPLICATION_CONTEXT ( 'automotive_design' ) ;
#695 = VECTOR ( 'NONE', #7305, 1000.000000000000000 ) ;
#696 = CIRCLE ( 'NONE', #6850, 4.999999999999997335 ) ;
#697 = CIRCLE ( 'NONE', #1462, 5.000000000000000000 ) ;
#698 = VERTEX_POINT ( 'NONE', #733 ) ;
#699 = EDGE_LOOP ( 'NONE', ( #2725, #2849, #4765, #6053 ) ) ;
#700 = LINE ( 'NONE', #3155, #3685 ) ;
#701 = DIRECTION ( 'NONE',  ( -0.000000000000000000, -0.000000000000000000, -1.000000000000000000 ) ) ;
#703 = DIRECTION ( 'NONE',  ( 0.000000000000000000, 0.000000000000000000, -1.000000000000000000 ) ) ;
#702 = VECTOR ( 'NONE', #6970, 1000.000000000000000 ) ;
#704 = AXIS2_PLACEMENT_3D ( 'NONE', #5018, #167, #210 ) ;
#705 = DIRECTION ( 'NONE',  ( -1.000000000000000000, 0.000000000000000000, 0.000000000000000000 ) ) ;
#706 = ORIENTED_EDGE ( 'NONE', *, *, #2407, .F. ) ;
#707 = DIRECTION ( 'NONE',  ( 0.000000000000000000, 0.000000000000000000, -1.000000000000000000 ) ) ;
#708 = UNCERTAINTY_MEASURE_WITH_UNIT (LENGTH_MEASURE( 1.000000000000000082E-05 ), #6956, 'distance_accuracy_value', 'NONE');
#709 = AXIS2_PLACEMENT_3D ( 'NONE', #7627, #5212, #2824 ) ;
#710 = DIRECTION ( 'NONE',  ( -1.000000000000000000, -0.000000000000000000, -0.000000000000000000 ) ) ;
#711 = ORIENTED_EDGE ( 'NONE', *, *, #3197, .F. ) ;
#712 = CARTESIAN_POINT ( 'NONE',  ( 0.000000000000000000, 0.000000000000000000, 1.000000000000028644 ) ) ;
#713 = ORIENTED_EDGE ( 'NONE', *, *, #134, .T. ) ;
#714 = DIRECTION ( 'NONE',  ( -0.5000000000000003331, 0.8660254037844383745, 0.000000000000000000 ) ) ;
#715 = CIRCLE ( 'NONE', #2641, 12.50000000000001066 ) ;
#716 = LINE ( 'NONE', #3209, #7756 ) ;
#717 = EDGE_CURVE ( 'NONE', #1167, #7818, #2890, .T. ) ;
#718 = EDGE_CURVE ( 'NONE', #1234, #1377, #2427, .T. ) ;
#719 = ORIENTED_EDGE ( 'NONE', *, *, #6111, .F. ) ;
#720 =( GEOMETRIC_REPRESENTATION_CONTEXT ( 3 ) GLOBAL_UNCERTAINTY_ASSIGNED_CONTEXT ( ( #708 ) ) GLOBAL_UNIT_ASSIGNED_CONTEXT ( ( #6956, #5552, #3868 ) ) REPRESENTATION_CONTEXT ( 'NONE', 'WORKASPACE' ) );
#721 = ORIENTED_EDGE ( 'NONE', *, *, #3608, .F. ) ;
#722 = ORIENTED_EDGE ( 'NONE', *, *, #1940, .T. ) ;
#723 = DIRECTION ( 'NONE',  ( 1.000000000000000000, 0.000000000000000000, 0.000000000000000000 ) ) ;
#724 = EDGE_CURVE ( 'NONE', #5251, #1704, #131, .T. ) ;
#725 = CARTESIAN_POINT ( 'NONE',  ( 386.6633783623262843, -19.48763309926589216, -4.514690562563614229 ) ) ;
#726 = DIRECTION ( 'NONE',  ( 0.000000000000000000, 0.000000000000000000, -1.000000000000000000 ) ) ;
#727 = CARTESIAN_POINT ( 'NONE',  ( 296.6025403784437913, 135.0000000000000000, 12.50000000000000000 ) ) ;
#728 = DIRECTION ( 'NONE',  ( -1.000000000000000000, 4.270088556250607616E-16, -0.000000000000000000 ) ) ;
#729 =( GEOMETRIC_REPRESENTATION_CONTEXT ( 3 ) GLOBAL_UNCERTAINTY_ASSIGNED_CONTEXT ( ( #386 ) ) GLOBAL_UNIT_ASSIGNED_CONTEXT ( ( #2222, #335, #7676 ) ) REPRESENTATION_CONTEXT ( 'NONE', 'WORKASPACE' ) );
#730 = CIRCLE ( 'NONE', #861, 25.00000003264134918 ) ;
#731 = LINE ( 'NONE', #7435, #7643 ) ;
#732 = PLANE ( 'NONE',  #7801 ) ;
#733 = CARTESIAN_POINT ( 'NONE',  ( -12.50000000000000000, 0.000000000000000000, 0.000000000000000000 ) ) ;
#734 = FACE_OUTER_BOUND ( 'NONE', #2970, .T. ) ;
#735 = EDGE_CURVE ( 'NONE', #389, #387, #1592, .T. ) ;
#736 = CIRCLE ( 'NONE', #7274, 25.00000000000000000 ) ;
#737 = ORIENTED_EDGE ( 'NONE', *, *, #4235, .F. ) ;
#738 = ORIENTED_EDGE ( 'NONE', *, *, #787, .T. ) ;
#739 = AXIS2_PLACEMENT_3D ( 'NONE', #5978, #5900, #1078 ) ;
#740 = FILL_AREA_STYLE_COLOUR ( '', #332 ) ;
#741 = DIRECTION ( 'NONE',  ( -1.000000000000000000, 0.000000000000000000, 0.000000000000000000 ) ) ;
#742 = AXIS2_PLACEMENT_3D ( 'NONE', #2433, #7878, #7098 ) ;
#743 = DIRECTION ( 'NONE',  ( 1.000000000000000000, 0.000000000000000000, 0.000000000000000000 ) ) ;
#744 = CARTESIAN_POINT ( 'NONE',  ( 72.36967921662629522, 50.20544122544588816, 0.000000000000000000 ) ) ;
#745 = ORIENTED_EDGE ( 'NONE', *, *, #6400, .T. ) ;
#746 = CYLINDRICAL_SURFACE ( 'NONE', #5836, 5.000000000000000888 ) ;
#747 = VECTOR ( 'NONE', #254, 1000.000000000000000 ) ;
#748 = CARTESIAN_POINT ( 'NONE',  ( 372.0982571448921590, 15.87479745381989815, -12.16559770555248754 ) ) ;
#749 = EDGE_LOOP ( 'NONE', ( #6564, #6414, #6580, #3207 ) ) ;
#750 = CYLINDRICAL_SURFACE ( 'NONE', #3535, 12.50000000000000000 ) ;
#751 = ORIENTED_EDGE ( 'NONE', *, *, #1464, .T. ) ;
#752 = AXIS2_PLACEMENT_3D ( 'NONE', #4614, #4175, #7158 ) ;
#753 = CARTESIAN_POINT ( 'NONE',  ( -12.50000000000000000, 0.000000000000000000, 75.00000000000000000 ) ) ;
#754 = CIRCLE ( 'NONE', #5883, 12.50000000000000355 ) ;
#755 = CARTESIAN_POINT ( 'NONE',  ( 11.49999999999995914, 0.000000000000000000, 0.000000000000000000 ) ) ;
#756 = VERTEX_POINT ( 'NONE', #7471 ) ;
#757 = AXIS2_PLACEMENT_3D ( 'NONE', #1518, #3404, #5810 ) ;
#758 = AXIS2_PLACEMENT_3D ( 'NONE', #6542, #5289, #4124 ) ;
#759 = ORIENTED_EDGE ( 'NONE', *, *, #6177, .F. ) ;
#760 = EDGE_CURVE ( 'NONE', #2724, #6891, #6193, .T. ) ;
#761 = ORIENTED_EDGE ( 'NONE', *, *, #2422, .T. ) ;
#762 = CARTESIAN_POINT ( 'NONE',  ( -12.50000000000000000, 25.00000000000000000, 0.000000000000000000 ) ) ;
#763 = CARTESIAN_POINT ( 'NONE',  ( 375.0000000000000000, -15.61249499599599488, -12.50000000000000000 ) ) ;
#764 = ORIENTED_EDGE ( 'NONE', *, *, #7360, .F. ) ;
#765 = EDGE_CURVE ( 'NONE', #2601, #6545, #620, .T. ) ;
#766 = CARTESIAN_POINT ( 'NONE',  ( 6.602357126051254174E-16, 0.000000000000000000, 0.000000000000000000 ) ) ;
#767 = CONTEXT_DEPENDENT_SHAPE_REPRESENTATION ( #4590, #7206 ) ;
#768 = DIRECTION ( 'NONE',  ( 0.000000000000000000, -0.000000000000000000, 1.000000000000000000 ) ) ;
#769 = CARTESIAN_POINT ( 'NONE',  ( -4.731064025391297956E-15, 37.50000000000004263, 12.50000000000000000 ) ) ;
#770 = CARTESIAN_POINT ( 'NONE',  ( 42.50000000000000000, 37.50000000000003553, 12.50000000000000000 ) ) ;
#771 = LINE ( 'NONE', #3225, #4156 ) ;
#772 = B_SPLINE_CURVE_WITH_KNOTS ( 'NONE', 3,
 ( #7335, #1945, #6284, #748, #27, #4429, #64, #1312, #2476, #6208, #3237, #3801, #1827, #1387, #3691, #5565, #3163, #3204, #5648, #2558, #3733, #148, #7375, #2441, #4387, #6727, #5030, #5000, #1987, #7452, #6849, #6888, #4876, #3839, #2516, #7414, #785, #5685, #4957, #1912, #1235, #6170, #6130, #639, #3091, #5528, #1277, #4915, #1868, #4315 ),
 .UNSPECIFIED., .F., .F.,
 ( 4, 2, 2, 2, 2, 2, 2, 2, 2, 2, 2, 2, 2, 2, 2, 2, 2, 2, 2, 2, 2, 2, 2, 2, 4 ),
 ( 0.000000000000000000, 0.002511627799209755017, 0.003767441698814711672, 0.005023255598419669628, 0.007534883397629582938, 0.01004651119683949712, 0.01130232509644451058, 0.01255813899604952405, 0.01506976679525946078, 0.01632558069486442914, 0.01758139459446940098, 0.02009302239367936893, 0.02134883629328435117, 0.02260465019288934035, 0.02386046409249432260, 0.02511627799209930484, 0.02762790579130921381, 0.03013953359051911585, 0.03139534749012407033, 0.03265116138972902482, 0.03516278918893894073, 0.03641860308854381889, 0.03767441698814869705, 0.03893023088775358215, 0.04018604478735846031 ),
 .UNSPECIFIED. ) ;
#773 = ORIENTED_EDGE ( 'NONE', *, *, #4377, .T. ) ;
#774 = CARTESIAN_POINT ( 'NONE',  ( 398.6828372460798846, -12.50000000000000000, -14.73776325548316812 ) ) ;
#775 = EDGE_LOOP ( 'NONE', ( #3337, #854 ) ) ;
#776 = EDGE_CURVE ( 'NONE', #6431, #2724, #3901, .T. ) ;
#777 = CARTESIAN_POINT ( 'NONE',  ( 18.76388374866283471, -1.044563157018773529E-16, 7.500000000000000000 ) ) ;
#778 = CARTESIAN_POINT ( 'NONE',  ( -4.731064025391297956E-15, 37.50000000000004263, 12.50000000000000000 ) ) ;
#779 = CARTESIAN_POINT ( 'NONE',  ( 6.602357126051254174E-16, 0.000000000000000000, 0.000000000000000000 ) ) ;
#780 = CARTESIAN_POINT ( 'NONE',  ( 232.4759526419164217, 243.7500000000000000, 0.000000000000000000 ) ) ;
#781 = VERTEX_POINT ( 'NONE', #3716 ) ;
#782 = AXIS2_PLACEMENT_3D ( 'NONE', #3942, #3383, #172 ) ;
#783 = UNCERTAINTY_MEASURE_WITH_UNIT (LENGTH_MEASURE( 1.000000000000000082E-05 ), #590, 'distance_accuracy_value', 'NONE');
#784 = VERTEX_POINT ( 'NONE', #3111 ) ;
#785 = CARTESIAN_POINT ( 'NONE',  ( 366.7510386178572048, 17.65558712887547443, 9.400222409301415283 ) ) ;
#786 = ORIENTED_EDGE ( 'NONE', *, *, #483, .F. ) ;
#787 = EDGE_CURVE ( 'NONE', #756, #6450, #697, .T. ) ;
#788 = CARTESIAN_POINT ( 'NONE',  ( 296.6025403784439050, 75.00000000000007105, 5.000000000000000000 ) ) ;
#789 = ORIENTED_EDGE ( 'NONE', *, *, #7829, .F. ) ;
#790 = CARTESIAN_POINT ( 'NONE',  ( 0.000000000000000000, 0.000000000000000000, 195.9999999999999716 ) ) ;
#791 = CARTESIAN_POINT ( 'NONE',  ( 0.000000000000000000, 262.5000000000000568, 12.50000000000000000 ) ) ;
#792 = VERTEX_POINT ( 'NONE', #4862 ) ;
#793 = CARTESIAN_POINT ( 'NONE',  ( 0.000000000000000000, 0.000000000000000000, 2.000000000000001776 ) ) ;
#794 = ORIENTED_EDGE ( 'NONE', *, *, #567, .F. ) ;
#795 = ORIENTED_EDGE ( 'NONE', *, *, #3102, .T. ) ;
#796 = DIRECTION ( 'NONE',  ( 0.000000000000000000, 0.000000000000000000, 1.000000000000000000 ) ) ;
#797 = CARTESIAN_POINT ( 'NONE',  ( 340.0000000000000000, 12.50000000000000000, 15.61249499599599488 ) ) ;
#798 = DIRECTION ( 'NONE',  ( -0.7071067811865479058, 0.000000000000000000, 0.7071067811865472397 ) ) ;
#799 = ORIENTED_EDGE ( 'NONE', *, *, #5542, .T. ) ;
#800 = CARTESIAN_POINT ( 'NONE',  ( -12.50000000000000355, 1.530808498934191916E-15, 92.50000000000000000 ) ) ;
#801 = PRODUCT_RELATED_PRODUCT_CATEGORY ( 'part', '', ( #3221 ) ) ;
#802 = VECTOR ( 'NONE', #5540, 1000.000000000000000 ) ;
#803 = EDGE_CURVE ( 'NONE', #3524, #2004, #5949, .T. ) ;
#804 = ITEM_DEFINED_TRANSFORMATION ( 'NONE', 'NONE', #4622,  #5785 ) ;
#805 = DIRECTION ( 'NONE',  ( -4.789677997474686366E-16, -1.000000000000000000, -0.000000000000000000 ) ) ;
#806 = LINE ( 'NONE', #1444, #7164 ) ;
#807 = DIRECTION ( 'NONE',  ( 0.000000000000000000, -0.000000000000000000, 1.000000000000000000 ) ) ;
#808 = DIRECTION ( 'NONE',  ( 0.000000000000000000, 0.000000000000000000, -1.000000000000000000 ) ) ;
#809 = EDGE_CURVE ( 'NONE', #1302, #4126, #3780, .T. ) ;
#810 = EDGE_CURVE ( 'NONE', #52, #5747, #3752, .T. ) ;
#811 = ORIENTED_EDGE ( 'NONE', *, *, #6848, .F. ) ;
#812 = CIRCLE ( 'NONE', #4650, 25.00000000000000711 ) ;
#813 = DIRECTION ( 'NONE',  ( -0.000000000000000000, -0.000000000000000000, -1.000000000000000000 ) ) ;
#814 = SHAPE_REPRESENTATION_RELATIONSHIP ( 'NONE' , 'NONE' ,  #341, #3928 ) ;
#815 = ORIENTED_EDGE ( 'NONE', *, *, #6606, .F. ) ;
#816 = DIRECTION ( 'NONE',  ( -1.000000000000000000, -0.000000000000000000, -0.000000000000000000 ) ) ;
#817 = LINE ( 'NONE', #6477, #6078 ) ;
#818 = DIRECTION ( 'NONE',  ( -0.000000000000000000, -0.000000000000000000, -1.000000000000000000 ) ) ;
#819 = VERTEX_POINT ( 'NONE', #1371 ) ;
#820 = EDGE_CURVE ( 'NONE', #1377, #6439, #6344, .T. ) ;
#821 = AXIS2_PLACEMENT_3D ( 'NONE', #7617, #1562, #921 ) ;
#822 = AXIS2_PLACEMENT_3D ( 'NONE', #6595, #6523, #7239 ) ;
#823 = ORIENTED_EDGE ( 'NONE', *, *, #5572, .F. ) ;
#824 = VECTOR ( 'NONE', #32, 1000.000000000000000 ) ;
#825 = CARTESIAN_POINT ( 'NONE',  ( -12.50000000000000000, 1.530808498934191521E-15, 1.000000000000028644 ) ) ;
#826 = PRESENTATION_LAYER_ASSIGNMENT (  '', '', ( #4283 ) ) ;
#827 = ORIENTED_EDGE ( 'NONE', *, *, #6507, .T. ) ;
#828 = VECTOR ( 'NONE', #1297, 1000.000000000000000 ) ;
#829 = DIRECTION ( 'NONE',  ( -1.000000000000000000, 0.000000000000000000, 0.000000000000000000 ) ) ;
#830 = DIRECTION ( 'NONE',  ( 0.000000000000000000, 0.000000000000000000, 1.000000000000000000 ) ) ;
#831 = FACE_BOUND ( 'NONE', #990, .T. ) ;
#832 = FACE_OUTER_BOUND ( 'NONE', #4118, .T. ) ;
#833 = VECTOR ( 'NONE', #6443, 1000.000000000000000 ) ;
#834 = ADVANCED_FACE ( 'NONE', ( #7587 ), #6949, .T. ) ;
#835 = ORIENTED_EDGE ( 'NONE', *, *, #7339, .T. ) ;
#836 = CARTESIAN_POINT ( 'NONE',  ( 412.4999999999998863, 137.4999999999999716, 12.50000000000000000 ) ) ;
#837 = ORIENTED_EDGE ( 'NONE', *, *, #6507, .F. ) ;
#838 = VECTOR ( 'NONE', #145, 1000.000000000000000 ) ;
#839 = EDGE_LOOP ( 'NONE', ( #5596, #2921, #2429, #1231 ) ) ;
#840 = DIRECTION ( 'NONE',  ( 0.000000000000000000, 0.000000000000000000, 1.000000000000000000 ) ) ;
#841 = FILL_AREA_STYLE_COLOUR ( '', #7103 ) ;
#842 = CARTESIAN_POINT ( 'NONE',  ( 412.5000000000000568, 142.5000000000000000, 20.00000000000000000 ) ) ;
#843 = EDGE_LOOP ( 'NONE', ( #7455, #2077, #860, #494 ) ) ;
#844 = DIRECTION ( 'NONE',  ( -0.000000000000000000, -0.000000000000000000, -1.000000000000000000 ) ) ;
#845 = CONICAL_SURFACE ( 'NONE', #5330, 12.50000000000000000, 0.7853981633974543852 ) ;
#846 = VERTEX_POINT ( 'NONE', #6914 ) ;
#847 = CARTESIAN_POINT ( 'NONE',  ( 1.320471425210250835E-15, 0.000000000000000000, 25.00000000000000000 ) ) ;
#848 = CARTESIAN_POINT ( 'NONE',  ( -25.00000000000000000, 25.00000000000000000, 0.000000000000000000 ) ) ;
#849 = CARTESIAN_POINT ( 'NONE',  ( -74.28095588234631919, 0.000000000000000000, 12.50000000000000000 ) ) ;
#850 = CARTESIAN_POINT ( 'NONE',  ( 3.081487911019577803E-31, -25.00000000000000355, 37.50000000000000000 ) ) ;
#851 = ORIENTED_EDGE ( 'NONE', *, *, #7776, .T. ) ;
#852 = VECTOR ( 'NONE', #1540, 1000.000000000000000 ) ;
#853 = CARTESIAN_POINT ( 'NONE',  ( -250.9131605378006498, 164.1990734970207200, 183.2402661832477406 ) ) ;
#854 = ORIENTED_EDGE ( 'NONE', *, *, #6480, .F. ) ;
#855 = EDGE_CURVE ( 'NONE', #7362, #1918, #6307, .T. ) ;
#856 = CARTESIAN_POINT ( 'NONE',  ( -36.78095584970496645, 12.70544120911856290, 12.50000000000000000 ) ) ;
#857 = CARTESIAN_POINT ( 'NONE',  ( 412.5000000000002274, 1.221245327087672598E-12, 12.50000000000000000 ) ) ;
#858 = DIRECTION ( 'NONE',  ( 1.000000000000000000, 0.000000000000000000, 0.000000000000000000 ) ) ;
#859 = CARTESIAN_POINT ( 'NONE',  ( 190.0000000000000000, 3.061616997868383043E-15, -25.00000000000000000 ) ) ;
#860 = ORIENTED_EDGE ( 'NONE', *, *, #470, .F. ) ;
#861 = AXIS2_PLACEMENT_3D ( 'NONE', #1725, #3660, #4213 ) ;
#862 = EDGE_CURVE ( 'NONE', #7501, #642, #7108, .T. ) ;
#863 = ORIENTED_EDGE ( 'NONE', *, *, #7066, .F. ) ;
#864 = EDGE_CURVE ( 'NONE', #5496, #5551, #2131, .T. ) ;
#865 = ADVANCED_FACE ( 'NONE', ( #7030 ), #288, .F. ) ;
#866 = DIRECTION ( 'NONE',  ( -1.000000000000000000, -0.000000000000000000, -0.000000000000000000 ) ) ;
#867 = ORIENTED_EDGE ( 'NONE', *, *, #3488, .F. ) ;
#868 = CARTESIAN_POINT ( 'NONE',  ( -8.959197987552832032, 23.33951095074251114, 25.00000000000000000 ) ) ;
#869 = VERTEX_POINT ( 'NONE', #4497 ) ;
#870 = DIRECTION ( 'NONE',  ( 0.000000000000000000, -0.000000000000000000, 1.000000000000000000 ) ) ;
#871 = LINE ( 'NONE', #3326, #586 ) ;
#872 = CIRCLE ( 'NONE', #1773, 15.64999999999999680 ) ;
#873 = AXIS2_PLACEMENT_3D ( 'NONE', #1597, #2393, #1524 ) ;
#874 = ORIENTED_EDGE ( 'NONE', *, *, #4882, .F. ) ;
#875 = CARTESIAN_POINT ( 'NONE',  ( -25.00000000000000000, 0.000000000000000000, -12.50000000000000000 ) ) ;
#876 = ORIENTED_EDGE ( 'NONE', *, *, #101, .F. ) ;
#877 = AXIS2_PLACEMENT_3D ( 'NONE', #4636, #3286, #1593 ) ;
#878 = AXIS2_PLACEMENT_3D ( 'NONE', #7202, #7715, #1699 ) ;
#879 = ORIENTED_EDGE ( 'NONE', *, *, #2053, .F. ) ;
#880 = CARTESIAN_POINT ( 'NONE',  ( 340.0000000000000000, 0.000000000000000000, 0.000000000000000000 ) ) ;
#881 = ADVANCED_FACE ( 'NONE', ( #6427 ), #5096, .F. ) ;
#882 = DIRECTION ( 'NONE',  ( -0.000000000000000000, 0.000000000000000000, 1.000000000000000000 ) ) ;
#883 = CARTESIAN_POINT ( 'NONE',  ( 52.50000000000000711, 177.5000000000000000, 130.0000000000000000 ) ) ;
#884 = DIRECTION ( 'NONE',  ( -0.000000000000000000, -0.000000000000000000, -1.000000000000000000 ) ) ;
#885 = CIRCLE ( 'NONE', #371, 5.000000000000004441 ) ;
#886 = VERTEX_POINT ( 'NONE', #2697 ) ;
#887 = ITEM_DEFINED_TRANSFORMATION ( 'NONE', 'NONE', #2976,  #5785 ) ;
#888 = CARTESIAN_POINT ( 'NONE',  ( 340.0000000000000000, -12.50000000000000355, 21.65063509461096558 ) ) ;
#889 = PLANE ( 'NONE',  #4085 ) ;
#890 = CARTESIAN_POINT ( 'NONE',  ( 0.000000000000000000, 113.0000000000000995, 130.0000000000000000 ) ) ;
#891 = DIRECTION ( 'NONE',  ( -1.000000000000000000, -0.000000000000000000, -0.000000000000000000 ) ) ;
#892 = DIRECTION ( 'NONE',  ( 0.8886649088774987160, 0.4585571717133501424, -0.000000000000000000 ) ) ;
#893 = CARTESIAN_POINT ( 'NONE',  ( -11.78095584970496290, 62.70544120911855401, 12.50000000000000000 ) ) ;
#894 = EDGE_LOOP ( 'NONE', ( #2327, #6080 ) ) ;
#895 = CARTESIAN_POINT ( 'NONE',  ( 137.4999999999999716, 1.836970198721029747E-14, 0.000000000000000000 ) ) ;
#896 = DIRECTION ( 'NONE',  ( 0.000000000000000000, -0.000000000000000000, -1.000000000000000000 ) ) ;
#897 = PLANE ( 'NONE',  #6204 ) ;
#898 = DIRECTION ( 'NONE',  ( 0.000000000000000000, -0.000000000000000000, 1.000000000000000000 ) ) ;
#899 = EDGE_LOOP ( 'NONE', ( #6972, #5043, #1433, #7453 ) ) ;
#900 = EDGE_CURVE ( 'NONE', #968, #1507, #4611, .T. ) ;
#901 =( REPRESENTATION_RELATIONSHIP ('NONE','NONE', #6292, #3730 ) REPRESENTATION_RELATIONSHIP_WITH_TRANSFORMATION ( #3072 )SHAPE_REPRESENTATION_RELATIONSHIP( ) );
#902 = ORIENTED_EDGE ( 'NONE', *, *, #579, .F. ) ;
#903 = ADVANCED_FACE ( 'NONE', ( #5751 ), #3376, .T. ) ;
#904 = DIRECTION ( 'NONE',  ( 1.000000000000000000, 0.000000000000000000, 0.000000000000000000 ) ) ;
#905 = VERTEX_POINT ( 'NONE', #5668 ) ;
#906 = LINE ( 'NONE', #6440, #7257 ) ;
#907 = FACE_OUTER_BOUND ( 'NONE', #4552, .T. ) ;
#908 = CIRCLE ( 'NONE', #4747, 24.99999996734560881 ) ;
#909 =( NAMED_UNIT ( * ) PLANE_ANGLE_UNIT ( ) SI_UNIT ( $, .RADIAN. ) );
#910 = LINE ( 'NONE', #1586, #5309 ) ;
#911 = EDGE_CURVE ( 'NONE', #886, #5200, #2738, .T. ) ;
#912 = PRODUCT_DEFINITION_SHAPE ( 'NONE', 'NONE',  #7922 ) ;
#913 = PRODUCT_DEFINITION_FORMATION_WITH_SPECIFIED_SOURCE ( 'ANY', '', #2848, .NOT_KNOWN. ) ;
#914 = ORIENTED_EDGE ( 'NONE', *, *, #3379, .T. ) ;
#915 = LINE ( 'NONE', #3963, #2161 ) ;
#916 = VERTEX_POINT ( 'NONE', #5827 ) ;
#917 = DIRECTION ( 'NONE',  ( -0.000000000000000000, -0.000000000000000000, -1.000000000000000000 ) ) ;
#918 = ORIENTED_EDGE ( 'NONE', *, *, #1103, .T. ) ;
#919 = LINE ( 'NONE', #7058, #1634 ) ;
#920 = DIRECTION ( 'NONE',  ( -0.000000000000000000, -1.000000000000000000, -0.000000000000000000 ) ) ;
#921 = DIRECTION ( 'NONE',  ( 0.000000000000000000, 0.000000000000000000, 1.000000000000000000 ) ) ;
#922 = EDGE_LOOP ( 'NONE', ( #2515, #3791, #1468, #5188 ) ) ;
#923 = DIRECTION ( 'NONE',  ( -1.000000000000000000, 0.000000000000000000, 0.000000000000000000 ) ) ;
#924 = DIRECTION ( 'NONE',  ( -4.237492460401360996E-16, -1.000000000000000000, 0.000000000000000000 ) ) ;
#925 = CARTESIAN_POINT ( 'NONE',  ( 375.0000000000000000, 25.00000000000000000, 12.50000000000000711 ) ) ;
#926 = DIRECTION ( 'NONE',  ( 1.000000000000000000, 0.000000000000000000, 0.000000000000000000 ) ) ;
#927 = CARTESIAN_POINT ( 'NONE',  ( 377.9033602712955826, 15.87504132268115242, 12.16528391369894990 ) ) ;
#928 = EDGE_CURVE ( 'NONE', #5929, #1635, #5169, .T. ) ;
#929 = DIRECTION ( 'NONE',  ( -1.000000000000000000, -0.000000000000000000, -0.000000000000000000 ) ) ;
#930 = DIRECTION ( 'NONE',  ( -4.789677997474621285E-16, -1.000000000000000000, -3.608224830031758756E-16 ) ) ;
#931 = EDGE_LOOP ( 'NONE', ( #3127, #1836, #5610, #1028 ) ) ;
#932 = SURFACE_SIDE_STYLE ('',( #5834 ) ) ;
#933 = LINE ( 'NONE', #7559, #624 ) ;
#934 = CARTESIAN_POINT ( 'NONE',  ( 37.50000000000000711, 182.5000000000000000, 0.000000000000000000 ) ) ;
#935 = ORIENTED_EDGE ( 'NONE', *, *, #5561, .F. ) ;
#936 = VECTOR ( 'NONE', #4414, 1000.000000000000000 ) ;
#937 = UNCERTAINTY_MEASURE_WITH_UNIT (LENGTH_MEASURE( 1.000000000000000082E-05 ), #5795, 'distance_accuracy_value', 'NONE');
#938 = CLOSED_SHELL ( 'NONE', ( #3259, #881, #6446, #623, #2835, #6205, #3362, #7832, #625, #4608, #4436 ) ) ;
#939 = DIRECTION ( 'NONE',  ( -1.000000000000000000, 0.000000000000000000, -0.000000000000000000 ) ) ;
#940 = ORIENTED_EDGE ( 'NONE', *, *, #4377, .F. ) ;
#941 = CARTESIAN_POINT ( 'NONE',  ( 387.5000000000000568, 0.000000000000000000, 25.00000000000000000 ) ) ;
#943 = ORIENTED_EDGE ( 'NONE', *, *, #2332, .F. ) ;
#942 = VECTOR ( 'NONE', #3581, 1000.000000000000114 ) ;
#944 = VECTOR ( 'NONE', #4047, 1000.000000000000000 ) ;
#945 = AXIS2_PLACEMENT_3D ( 'NONE', #509, #7762, #2993 ) ;
#946 = EDGE_CURVE ( 'NONE', #4316, #7842, #5174, .T. ) ;
#947 = CYLINDRICAL_SURFACE ( 'NONE', #6520, 15.64999999999999680 ) ;
#948 = DIRECTION ( 'NONE',  ( -0.000000000000000000, -0.000000000000000000, -1.000000000000000000 ) ) ;
#949 = SHAPE_REPRESENTATION ( 'V-Link', ( #5785 ), #2447 ) ;
#950 = CIRCLE ( 'NONE', #3261, 15.00000000000000000 ) ;
#951 = VECTOR ( 'NONE', #1982, 1000.000000000000000 ) ;
#952 = ORIENTED_EDGE ( 'NONE', *, *, #2825, .T. ) ;
#953 = AXIS2_PLACEMENT_3D ( 'NONE', #7399, #1894, #4339 ) ;
#954 = DIRECTION ( 'NONE',  ( 1.000000000000000000, 0.000000000000000000, 0.000000000000000000 ) ) ;
#955 = EDGE_LOOP ( 'NONE', ( #17, #3274, #1865, #4677 ) ) ;
#956 = DIRECTION ( 'NONE',  ( 0.000000000000000000, 0.000000000000000000, -1.000000000000000000 ) ) ;
#957 = VERTEX_POINT ( 'NONE', #5131 ) ;
#958 = ADVANCED_BREP_SHAPE_REPRESENTATION ( '', ( #6795, #5785 ), #536 ) ;
#959 = CARTESIAN_POINT ( 'NONE',  ( -25.00000000000000000, 0.000000000000000000, 0.000000000000000000 ) ) ;
#960 = EDGE_CURVE ( 'NONE', #6891, #5142, #965, .T. ) ;
#961 = SURFACE_STYLE_USAGE ( .BOTH. , #5124 ) ;
#962 = DIRECTION ( 'NONE',  ( 1.000000000000000000, 0.000000000000000000, 0.000000000000000000 ) ) ;
#963 = AXIS2_PLACEMENT_3D ( 'NONE', #1645, #605, #1119 ) ;
#964 = CIRCLE ( 'NONE', #1601, 12.50000000000000355 ) ;
#965 = CIRCLE ( 'NONE', #5831, 5.000000000000000000 ) ;
#966 = CARTESIAN_POINT ( 'NONE',  ( -49.28095584970496645, 12.70544120911856112, 0.000000000000000000 ) ) ;
#967 = EDGE_CURVE ( 'NONE', #3100, #3167, #6092, .T. ) ;
#968 = VERTEX_POINT ( 'NONE', #5711 ) ;
#969 = CARTESIAN_POINT ( 'NONE',  ( 0.000000000000000000, 0.000000000000000000, 92.50000000000000000 ) ) ;
#970 = CARTESIAN_POINT ( 'NONE',  ( 75.00000000000000000, 10.56842436860067735, 25.00000000000000000 ) ) ;
#971 = DIRECTION ( 'NONE',  ( -0.000000000000000000, -0.000000000000000000, -1.000000000000000000 ) ) ;
#972 = DIRECTION ( 'NONE',  ( -0.000000000000000000, 0.000000000000000000, 1.000000000000000000 ) ) ;
#973 = CIRCLE ( 'NONE', #5457, 5.000000000000000888 ) ;
#974 = CARTESIAN_POINT ( 'NONE',  ( 385.7934419064004032, 18.97653311414304511, 6.355249004872655760 ) ) ;
#975 = DIRECTION ( 'NONE',  ( 1.000000000000000000, 0.000000000000000000, -0.000000000000000000 ) ) ;
#976 = AXIS2_PLACEMENT_3D ( 'NONE', #7211, #5517, #4905 ) ;
#977 = ORIENTED_EDGE ( 'NONE', *, *, #6848, .T. ) ;
#978 = CARTESIAN_POINT ( 'NONE',  ( 42.50000000000000000, 37.50000000000003553, 0.000000000000000000 ) ) ;
#979 = CARTESIAN_POINT ( 'NONE',  ( -20.00000000000000000, 0.000000000000000000, 47.50000000000000000 ) ) ;
#980 = EDGE_CURVE ( 'NONE', #2150, #3842, #7114, .T. ) ;
#981 = DIRECTION ( 'NONE',  ( 0.000000000000000000, -0.000000000000000000, -1.000000000000000000 ) ) ;
#982 = VERTEX_POINT ( 'NONE', #1489 ) ;
#983 = CIRCLE ( 'NONE', #6493, 5.000000000000004441 ) ;
#984 = ORIENTED_EDGE ( 'NONE', *, *, #1793, .F. ) ;
#985 = FACE_OUTER_BOUND ( 'NONE', #1432, .T. ) ;
#986 = ORIENTED_EDGE ( 'NONE', *, *, #3424, .T. ) ;
#987 = DIRECTION ( 'NONE',  ( 0.000000000000000000, 1.000000000000000000, 0.000000000000000000 ) ) ;
#988 = AXIS2_PLACEMENT_3D ( 'NONE', #324, #5863, #1565 ) ;
#989 = CARTESIAN_POINT ( 'NONE',  ( 3.831742397979759191E-14, 80.00000000000021316, 5.000000000000000000 ) ) ;
#990 = EDGE_LOOP ( 'NONE', ( #1605, #7138 ) ) ;
#991 = DIRECTION ( 'NONE',  ( -0.000000000000000000, -0.000000000000000000, -1.000000000000000000 ) ) ;
#992 = DIRECTION ( 'NONE',  ( -0.000000000000000000, 0.000000000000000000, 1.000000000000000000 ) ) ;
#993 = AXIS2_PLACEMENT_3D ( 'NONE', #7347, #6223, #1883 ) ;
#994 = VERTEX_POINT ( 'NONE', #7069 ) ;
#995 = CARTESIAN_POINT ( 'NONE',  ( -12.50000000000000000, 25.00000000000000355, 3.703880899869785475E-15 ) ) ;
#996 = EDGE_LOOP ( 'NONE', ( #6726, #6202, #7641, #4101 ) ) ;
#997 = EDGE_CURVE ( 'NONE', #1382, #7382, #7753, .T. ) ;
#998 = LINE ( 'NONE', #4122, #3408 ) ;
#999 = EDGE_LOOP ( 'NONE', ( #5153, #5490, #4822, #6178 ) ) ;
#1000 = CARTESIAN_POINT ( 'NONE',  ( 0.000000000000000000, 0.000000000000000000, 75.00000000000000000 ) ) ;
#1001 = AXIS2_PLACEMENT_3D ( 'NONE', #1003, #488, #2856 ) ;
#1002 = DIRECTION ( 'NONE',  ( -0.000000000000000000, -0.000000000000000000, -1.000000000000000000 ) ) ;
#1003 = CARTESIAN_POINT ( 'NONE',  ( 182.4759526419164217, -105.3525403784438907, 12.50000000000000000 ) ) ;
#1004 = AXIS2_PLACEMENT_3D ( 'NONE', #1000, #5856, #4787 ) ;
#1005 = CARTESIAN_POINT ( 'NONE',  ( -17.32050807568877104, -2.499999999999999112, 7.500000000000000000 ) ) ;
#1006 = ORIENTED_EDGE ( 'NONE', *, *, #6028, .T. ) ;
#1007 = COLOUR_RGB ( '',0.7921568627450980005, 0.8196078431372548767, 0.9333333333333333481 ) ;
#1008 = EDGE_CURVE ( 'NONE', #4616, #792, #6217, .T. ) ;
#1009 = CIRCLE ( 'NONE', #1901, 32.75000000000000000 ) ;
#1010 = ORIENTED_EDGE ( 'NONE', *, *, #4531, .T. ) ;
#1011 = EDGE_CURVE ( 'NONE', #7344, #4687, #5447, .T. ) ;
#1012 = CARTESIAN_POINT ( 'NONE',  ( -17.50000000000000355, 0.000000000000000000, 90.00000000000000000 ) ) ;
#1013 = DIRECTION ( 'NONE',  ( -0.000000000000000000, -0.000000000000000000, -1.000000000000000000 ) ) ;
#1014 = DIRECTION ( 'NONE',  ( 1.000000000000000000, 0.000000000000000000, 0.000000000000000000 ) ) ;
#1015 = CARTESIAN_POINT ( 'NONE',  ( 12.50000000000002309, 225.0000000000000284, 0.000000000000000000 ) ) ;
#1016 = CIRCLE ( 'NONE', #3076, 5.000000000000004441 ) ;
#1017 = CARTESIAN_POINT ( 'NONE',  ( 0.000000000000000000, 87.50000000000005684, 12.50000000000000000 ) ) ;
#1018 = EDGE_CURVE ( 'NONE', #4785, #4458, #2374, .T. ) ;
#1019 = DIRECTION ( 'NONE',  ( -0.000000000000000000, 0.000000000000000000, 1.000000000000000000 ) ) ;
#1020 = VECTOR ( 'NONE', #3603, 1000.000000000000000 ) ;
#1021 = PRODUCT_CONTEXT ( 'NONE', #133, 'mechanical' ) ;
#1022 = EDGE_LOOP ( 'NONE', ( #5127, #3440, #6797, #1983 ) ) ;
#1023 = DIRECTION ( 'NONE',  ( -0.000000000000000000, -0.000000000000000000, -1.000000000000000000 ) ) ;
#1024 = CARTESIAN_POINT ( 'NONE',  ( 0.000000000000000000, 0.000000000000000000, 47.50000000000000000 ) ) ;
#1025 = CARTESIAN_POINT ( 'NONE',  ( -49.28095584970496645, -62.29455879088143888, 12.50000000000000000 ) ) ;
#1026 = ORIENTED_EDGE ( 'NONE', *, *, #4143, .F. ) ;
#1027 = EDGE_CURVE ( 'NONE', #6360, #4316, #3580, .T. ) ;
#1028 = ORIENTED_EDGE ( 'NONE', *, *, #5917, .F. ) ;
#1029 =( LENGTH_UNIT ( ) NAMED_UNIT ( * ) SI_UNIT ( .MILLI., .METRE. ) );
#1030 = ORIENTED_EDGE ( 'NONE', *, *, #1181, .F. ) ;
#1031 = FILL_AREA_STYLE_COLOUR ( '', #6873 ) ;
#1032 = FACE_OUTER_BOUND ( 'NONE', #899, .T. ) ;
#1033 = ORIENTED_EDGE ( 'NONE', *, *, #2037, .F. ) ;
#1034 = PLANE ( 'NONE',  #3570 ) ;
#1035 = DIRECTION ( 'NONE',  ( -1.000000000000000000, 0.000000000000000000, 0.000000000000000000 ) ) ;
#1036 = VERTEX_POINT ( 'NONE', #4095 ) ;
#1037 = EDGE_CURVE ( 'NONE', #2505, #2977, #192, .T. ) ;
#1038 = LINE ( 'NONE', #4678, #3582 ) ;
#1039 = EDGE_LOOP ( 'NONE', ( #3039, #1762 ) ) ;
#1040 = CARTESIAN_POINT ( 'NONE',  ( 41.25000000000002842, 47.34122918275932079, 12.50000000000000000 ) ) ;
#1041 = ORIENTED_EDGE ( 'NONE', *, *, #364, .F. ) ;
#1042 = CARTESIAN_POINT ( 'NONE',  ( -24.28095581706362083, -62.29455879088143888, 12.50000000000000000 ) ) ;
#1043 = FACE_OUTER_BOUND ( 'NONE', #7603, .T. ) ;
#1044 = CARTESIAN_POINT ( 'NONE',  ( -37.49999999999992184, 113.0000000000000995, 130.0000000000000000 ) ) ;
#1045 = EDGE_LOOP ( 'NONE', ( #431, #6652, #298, #626 ) ) ;
#1046 = ORIENTED_EDGE ( 'NONE', *, *, #3653, .F. ) ;
#1047 = FACE_BOUND ( 'NONE', #5656, .T. ) ;
#1048 = DIRECTION ( 'NONE',  ( -0.000000000000000000, -0.000000000000000000, -1.000000000000000000 ) ) ;
#1049 = CARTESIAN_POINT ( 'NONE',  ( 0.000000000000000000, 0.000000000000000000, 25.00000000000000000 ) ) ;
#1050 = CARTESIAN_POINT ( 'NONE',  ( 12.50000000000000000, -25.00000000000000355, 37.50000000000000000 ) ) ;
#1051 = DIRECTION ( 'NONE',  ( 0.5000000000000000000, 0.8660254037844385966, 0.000000000000000000 ) ) ;
#1052 = EDGE_CURVE ( 'NONE', #7745, #2331, #454, .T. ) ;
#1053 = DIRECTION ( 'NONE',  ( -0.000000000000000000, 0.000000000000000000, 1.000000000000000000 ) ) ;
#1054 = DIRECTION ( 'NONE',  ( -4.789152899817899940E-16, -0.9999999999999998890, 4.157528252803118311E-20 ) ) ;
#1055 = ORIENTED_EDGE ( 'NONE', *, *, #323, .F. ) ;
#1056 = PLANE ( 'NONE',  #2027 ) ;
#1057 = CARTESIAN_POINT ( 'NONE',  ( 12.50000000000000000, 1.530808498934191521E-15, 0.5000000000000004441 ) ) ;
#1058 = ADVANCED_FACE ( 'NONE', ( #4733 ), #1090, .T. ) ;
#1059 = CARTESIAN_POINT ( 'NONE',  ( 0.000000000000000000, 0.000000000000000000, 12.50000000000000000 ) ) ;
#1060 = ORIENTED_EDGE ( 'NONE', *, *, #5526, .T. ) ;
#1061 = EDGE_CURVE ( 'NONE', #3356, #886, #6981, .T. ) ;
#1062 = EDGE_CURVE ( 'NONE', #905, #2195, #2108, .T. ) ;
#1063 = EDGE_LOOP ( 'NONE', ( #6818, #5603, #2310, #5112 ) ) ;
#1064 = VERTEX_POINT ( 'NONE', #2216 ) ;
#1065 = EDGE_CURVE ( 'NONE', #916, #3491, #6601, .T. ) ;
#1066 = EDGE_CURVE ( 'NONE', #7250, #1386, #7194, .T. ) ;
#1067 = CARTESIAN_POINT ( 'NONE',  ( 326.6025403784438481, 217.5000000000000284, 125.0000000000000000 ) ) ;
#1068 = ORIENTED_EDGE ( 'NONE', *, *, #4674, .T. ) ;
#1069 = PRESENTATION_STYLE_ASSIGNMENT (( #4116 ) ) ;
#1070 = LINE ( 'NONE', #479, #7244 ) ;
#1071 = AXIS2_PLACEMENT_3D ( 'NONE', #4710, #5925, #4113 ) ;
#1072 = EDGE_LOOP ( 'NONE', ( #4106, #5003, #4749, #4193 ) ) ;
#1073 = CARTESIAN_POINT ( 'NONE',  ( 15.64999999999999680, 1.916572240665607593E-15, 49.99999999999998579 ) ) ;
#1074 = ORIENTED_EDGE ( 'NONE', *, *, #5582, .T. ) ;
#1075 = VECTOR ( 'NONE', #6397, 1000.000000000000000 ) ;
#1076 = DIRECTION ( 'NONE',  ( 0.000000000000000000, -0.000000000000000000, -1.000000000000000000 ) ) ;
#1077 = ORIENTED_EDGE ( 'NONE', *, *, #1837, .T. ) ;
#1078 = DIRECTION ( 'NONE',  ( 0.000000000000000000, 0.000000000000000000, 1.000000000000000000 ) ) ;
#1079 = LINE ( 'NONE', #3610, #695 ) ;
#1080 = EDGE_CURVE ( 'NONE', #3053, #4682, #410, .T. ) ;
#1081 = CIRCLE ( 'NONE', #821, 32.75000000000000000 ) ;
#1082 = AXIS2_PLACEMENT_3D ( 'NONE', #1059, #5956, #2833 ) ;
#1083 = VECTOR ( 'NONE', #4571, 1000.000000000000000 ) ;
#1084 = ORIENTED_EDGE ( 'NONE', *, *, #5520, .F. ) ;
#1085 = ORIENTED_EDGE ( 'NONE', *, *, #1062, .F. ) ;
#1086 = AXIS2_PLACEMENT_3D ( 'NONE', #2762, #5149, #2035 ) ;
#1087 = AXIS2_PLACEMENT_3D ( 'NONE', #7280, #1854, #2957 ) ;
#1088 = CARTESIAN_POINT ( 'NONE',  ( 400.0000000000000568, 0.000000000000000000, 0.000000000000000000 ) ) ;
#1089 = CARTESIAN_POINT ( 'NONE',  ( 175.0000000000000000, 0.000000000000000000, 0.000000000000000000 ) ) ;
#1090 = PLANE ( 'NONE',  #1469 ) ;
#1091 = CARTESIAN_POINT ( 'NONE',  ( 63.21904415029505486, 62.70544120911855401, 12.50000000000000000 ) ) ;
#1092 = CARTESIAN_POINT ( 'NONE',  ( 75.00000000000000000, 55.56842436860067380, 25.00000000000000000 ) ) ;
#1093 = CIRCLE ( 'NONE', #461, 5.000000000000000888 ) ;
#1094 = CARTESIAN_POINT ( 'NONE',  ( -27.49999999999994671, 47.50000000000009237, 12.65877081724073783 ) ) ;
#1095 = DIRECTION ( 'NONE',  ( 1.000000000000000000, -4.789593822244094799E-16, -4.789593822244094799E-16 ) ) ;
#1096 = EDGE_LOOP ( 'NONE', ( #6058, #4187, #3905, #4902 ) ) ;
#1097 = CARTESIAN_POINT ( 'NONE',  ( 6.495190528383280260, 16.25000000000000000, 7.500000000000000000 ) ) ;
#1099 = FACE_OUTER_BOUND ( 'NONE', #3873, .T. ) ;
#1098 = AXIS2_PLACEMENT_3D ( 'NONE', #5651, #2596, #829 ) ;
#1100 = CARTESIAN_POINT ( 'NONE',  ( 0.000000000000000000, 0.000000000000000000, 12.50000000000000000 ) ) ;
#1101 = ORIENTED_EDGE ( 'NONE', *, *, #504, .T. ) ;
#1102 = VERTEX_POINT ( 'NONE', #2947 ) ;
#1103 = EDGE_CURVE ( 'NONE', #4697, #4272, #6184, .T. ) ;
#1104 = ORIENTED_EDGE ( 'NONE', *, *, #3636, .T. ) ;
#1105 = CARTESIAN_POINT ( 'NONE',  ( 325.0000000000000000, 0.000000000000000000, 0.000000000000000000 ) ) ;
#1106 = CARTESIAN_POINT ( 'NONE',  ( 25.00000000000000000, 24.99999999999999289, 50.00000000000000000 ) ) ;
#1107 = ADVANCED_FACE ( 'NONE', ( #535 ), #2863, .T. ) ;
#1108 = VERTEX_POINT ( 'NONE', #7792 ) ;
#1109 = AXIS2_PLACEMENT_3D ( 'NONE', #690, #3750, #5633 ) ;
#1110 = FACE_OUTER_BOUND ( 'NONE', #4157, .T. ) ;
#1111 = EDGE_CURVE ( 'NONE', #2565, #6642, #3466, .T. ) ;
#1112 = EDGE_LOOP ( 'NONE', ( #811, #5926, #6831, #2872 ) ) ;
#1113 = AXIS2_PLACEMENT_3D ( 'NONE', #5666, #805, #3255 ) ;
#1114 = PLANE ( 'NONE',  #7423 ) ;
#1115 = VERTEX_POINT ( 'NONE', #5906 ) ;
#1116 = CARTESIAN_POINT ( 'NONE',  ( 370.8902687158968092, -16.13982617348050752, -11.81224944216114459 ) ) ;
#1117 = VERTEX_POINT ( 'NONE', #413 ) ;
#1118 = DIRECTION ( 'NONE',  ( -1.000000000000000000, -4.789677997474691297E-16, 0.000000000000000000 ) ) ;
#1119 = DIRECTION ( 'NONE',  ( -1.000000000000000000, 0.000000000000000000, 0.000000000000000000 ) ) ;
#1120 = CIRCLE ( 'NONE', #2531, 25.00000000000000000 ) ;
#1121 = ORIENTED_EDGE ( 'NONE', *, *, #1545, .T. ) ;
#1122 = ORIENTED_EDGE ( 'NONE', *, *, #5838, .T. ) ;
#1123 = ADVANCED_FACE ( 'NONE', ( #5296 ), #2261, .T. ) ;
#1124 = AXIS2_PLACEMENT_3D ( 'NONE', #3011, #3737, #5570 ) ;
#1125 = VECTOR ( 'NONE', #4265, 1000.000000000000114 ) ;
#1126 = DIRECTION ( 'NONE',  ( -1.000000000000000000, 0.000000000000000000, 0.000000000000000000 ) ) ;
#1127 = CYLINDRICAL_SURFACE ( 'NONE', #4597, 17.50000000000000355 ) ;
#1128 = DIRECTION ( 'NONE',  ( 0.000000000000000000, 0.000000000000000000, 1.000000000000000000 ) ) ;
#1129 = LINE ( 'NONE', #8, #4910 ) ;
#1130 = CARTESIAN_POINT ( 'NONE',  ( 379.1097312841034181, 16.13982617348050752, -11.81224944216114459 ) ) ;
#1131 = AXIS2_PLACEMENT_3D ( 'NONE', #2016, #213, #1495 ) ;
#1132 = CIRCLE ( 'NONE', #3448, 12.50000000000000355 ) ;
#1133 = CARTESIAN_POINT ( 'NONE',  ( 0.000000000000000000, 0.000000000000000000, 92.50000000000000000 ) ) ;
#1134 = CARTESIAN_POINT ( 'NONE',  ( 364.5325195641692062, 194.6990734970207768, 283.9062424146593457 ) ) ;
#1135 = CIRCLE ( 'NONE', #506, 10.49999999999999467 ) ;
#1136 = PRESENTATION_STYLE_ASSIGNMENT (( #1735 ) ) ;
#1137 = FACE_OUTER_BOUND ( 'NONE', #6004, .T. ) ;
#1138 = AXIS2_PLACEMENT_3D ( 'NONE', #4103, #7761, #6634 ) ;
#1139 = DIRECTION ( 'NONE',  ( -1.000000000000000000, 0.000000000000000000, -0.000000000000000000 ) ) ;
#1140 = FACE_OUTER_BOUND ( 'NONE', #195, .T. ) ;
#1141 = VERTEX_POINT ( 'NONE', #5462 ) ;
#1142 = VECTOR ( 'NONE', #671, 1000.000000000000000 ) ;
#1143 = ORIENTED_EDGE ( 'NONE', *, *, #7483, .F. ) ;
#1144 = CIRCLE ( 'NONE', #2950, 5.000000000000000888 ) ;
#1145 = ORIENTED_EDGE ( 'NONE', *, *, #6739, .F. ) ;
#1146 =( LENGTH_UNIT ( ) NAMED_UNIT ( * ) SI_UNIT ( .MILLI., .METRE. ) );
#1147 = ORIENTED_EDGE ( 'NONE', *, *, #5859, .F. ) ;
#1148 = CARTESIAN_POINT ( 'NONE',  ( -12.50000000000000000, 0.000000000000000000, 0.000000000000000000 ) ) ;
#1149 = CARTESIAN_POINT ( 'NONE',  ( 0.000000000000000000, 0.000000000000000000, 25.00000000000000000 ) ) ;
#1150 = DIRECTION ( 'NONE',  ( 0.000000000000000000, 0.000000000000000000, -1.000000000000000000 ) ) ;
#1151 = LINE ( 'NONE', #5288, #6971 ) ;
#1152 = ORIENTED_EDGE ( 'NONE', *, *, #473, .F. ) ;
#1153 = DIRECTION ( 'NONE',  ( 0.000000000000000000, 0.000000000000000000, 1.000000000000000000 ) ) ;
#1154 = EDGE_CURVE ( 'NONE', #2477, #7188, #1886, .T. ) ;
#1155 = EDGE_CURVE ( 'NONE', #7046, #161, #3746, .T. ) ;
#1156 = ORIENTED_EDGE ( 'NONE', *, *, #101, .T. ) ;
#1157 = ADVANCED_FACE ( 'NONE', ( #82 ), #6147, .T. ) ;
#1158 = CARTESIAN_POINT ( 'NONE',  ( -17.32050807568877104, 2.500000000000002220, 7.500000000000000000 ) ) ;
#1159 = ORIENTED_EDGE ( 'NONE', *, *, #2526, .T. ) ;
#1160 = CARTESIAN_POINT ( 'NONE',  ( 364.4192847381275442, -18.85911174686545166, -6.667915149371354211 ) ) ;
#1161 = VERTEX_POINT ( 'NONE', #684 ) ;
#1162 = DIRECTION ( 'NONE',  ( -1.000000000000000000, -0.000000000000000000, -0.000000000000000000 ) ) ;
#1163 = EDGE_CURVE ( 'NONE', #1336, #1401, #3620, .T. ) ;
#1164 = DIRECTION ( 'NONE',  ( -1.000000000000000000, 0.000000000000000000, 0.000000000000000000 ) ) ;
#1165 = EDGE_CURVE ( 'NONE', #6439, #6276, #4254, .T. ) ;
#1166 = VERTEX_POINT ( 'NONE', #4975 ) ;
#1167 = VERTEX_POINT ( 'NONE', #4810 ) ;
#1168 = CARTESIAN_POINT ( 'NONE',  ( 383.5435001242829571, -17.79554561421092984, 9.133253117746194860 ) ) ;
#1169 = DIRECTION ( 'NONE',  ( -0.000000000000000000, -0.000000000000000000, -1.000000000000000000 ) ) ;
#1170 = CARTESIAN_POINT ( 'NONE',  ( 199.9999999999998863, 225.0000000000000284, 12.50000000000000000 ) ) ;
#1171 = DIRECTION ( 'NONE',  ( 0.000000000000000000, -0.000000000000000000, -1.000000000000000000 ) ) ;
#1172 = DIRECTION ( 'NONE',  ( 0.000000000000000000, 0.000000000000000000, -1.000000000000000000 ) ) ;
#1173 = DIRECTION ( 'NONE',  ( -1.000000000000000000, 0.000000000000000000, -0.000000000000000000 ) ) ;
#1174 = AXIS2_PLACEMENT_3D ( 'NONE', #1454, #5992, #2867 ) ;
#1175 = DIRECTION ( 'NONE',  ( 0.000000000000000000, -1.000000000000000000, 0.000000000000000000 ) ) ;
#1176 = APPLICATION_PROTOCOL_DEFINITION ( 'draft international standard', 'automotive_design', 1998, #6033 ) ;
#1177 = EDGE_CURVE ( 'NONE', #6088, #1102, #1769, .T. ) ;
#1178 = CARTESIAN_POINT ( 'NONE',  ( 286.6025403784437913, 0.000000000000000000, 12.50000000000000000 ) ) ;
#1179 = CARTESIAN_POINT ( 'NONE',  ( -17.50000000000000355, 0.000000000000000000, 97.50000000000000000 ) ) ;
#1180 = CARTESIAN_POINT ( 'NONE',  ( 0.000000000000000000, 0.000000000000000000, 75.00000000000000000 ) ) ;
#1181 = EDGE_CURVE ( 'NONE', #6545, #477, #6444, .T. ) ;
#1182 = ORIENTED_EDGE ( 'NONE', *, *, #4981, .F. ) ;
#1183 = ORIENTED_EDGE ( 'NONE', *, *, #7478, .T. ) ;
#1184 = CARTESIAN_POINT ( 'NONE',  ( 314.1025403784437913, 150.0000000000000568, 125.0000000000000000 ) ) ;
#1185 = CARTESIAN_POINT ( 'NONE',  ( 0.000000000000000000, 0.000000000000000000, 0.000000000000000000 ) ) ;
#1186 = LINE ( 'NONE', #2923, #5690 ) ;
#1187 = DIRECTION ( 'NONE',  ( -0.000000000000000000, 0.000000000000000000, 1.000000000000000000 ) ) ;
#1188 = EDGE_LOOP ( 'NONE', ( #3811, #2086 ) ) ;
#1189 = CARTESIAN_POINT ( 'NONE',  ( -0.000000000000000000, 47.50000000000003553, 0.000000000000000000 ) ) ;
#1190 = DIRECTION ( 'NONE',  ( -1.000000000000000000, 0.000000000000000000, 0.000000000000000000 ) ) ;
#1191 = ORIENTED_EDGE ( 'NONE', *, *, #5185, .T. ) ;
#1192 = PRODUCT_RELATED_PRODUCT_CATEGORY ( 'part', '', ( #2198 ) ) ;
#1193 = CARTESIAN_POINT ( 'NONE',  ( 373.3215647054732358, -15.68173745365923288, 12.41480524315420197 ) ) ;
#1194 = VERTEX_POINT ( 'NONE', #7900 ) ;
#1195 = FACE_BOUND ( 'NONE', #1713, .T. ) ;
#1196 = CARTESIAN_POINT ( 'NONE',  ( 50.71904415029504065, 62.70544120911855401, 12.50000000000000000 ) ) ;
#1197 = VECTOR ( 'NONE', #2659, 1000.000000000000000 ) ;
#1198 = ORIENTED_EDGE ( 'NONE', *, *, #7805, .F. ) ;
#1199 = AXIS2_PLACEMENT_3D ( 'NONE', #5771, #270, #2717 ) ;
#1200 = EDGE_LOOP ( 'NONE', ( #7084, #6403, #6235, #2079 ) ) ;
#1201 = ADVANCED_FACE ( 'NONE', ( #4367 ), #1325, .F. ) ;
#1202 = CARTESIAN_POINT ( 'NONE',  ( 338.3083524847281183, 217.5000000000000284, 168.7439889854708213 ) ) ;
#1203 = DIRECTION ( 'NONE',  ( 0.000000000000000000, -1.000000000000000000, 0.000000000000000000 ) ) ;
#1204 = DIRECTION ( 'NONE',  ( 0.000000000000000000, 0.000000000000000000, 1.000000000000000000 ) ) ;
#1205 = CARTESIAN_POINT ( 'NONE',  ( 41.66645320948619968, 177.5512430609197452, 12.50000000000000000 ) ) ;
#1206 = VECTOR ( 'NONE', #4255, 1000.000000000000114 ) ;
#1207 = EDGE_CURVE ( 'NONE', #2477, #4616, #6787, .T. ) ;
#1208 = CIRCLE ( 'NONE', #6844, 12.50000000000000355 ) ;
#1209 = DIRECTION ( 'NONE',  ( 1.000000000000000000, -1.387778780781445676E-15, 0.000000000000000000 ) ) ;
#1210 = CARTESIAN_POINT ( 'NONE',  ( 75.00000000000000000, 55.56842436860067380, 25.00000000000000000 ) ) ;
#1211 = EDGE_CURVE ( 'NONE', #1820, #1547, #428, .T. ) ;
#1212 = AXIS2_PLACEMENT_3D ( 'NONE', #3350, #7122, #5800 ) ;
#1213 = AXIS2_PLACEMENT_3D ( 'NONE', #7802, #2313, #4744 ) ;
#1214 = DIRECTION ( 'NONE',  ( 0.000000000000000000, -0.000000000000000000, 1.000000000000000000 ) ) ;
#1215 = CONTEXT_DEPENDENT_SHAPE_REPRESENTATION ( #1975, #7134 ) ;
#1216 = CARTESIAN_POINT ( 'NONE',  ( 6.602357126051254174E-16, 0.000000000000000000, 0.000000000000000000 ) ) ;
#1217 = DIRECTION ( 'NONE',  ( 0.000000000000000000, 0.000000000000000000, 1.000000000000000000 ) ) ;
#1218 = PLANE ( 'NONE',  #7750 ) ;
#1219 = DIRECTION ( 'NONE',  ( -1.000000000000000000, 0.000000000000000000, 0.000000000000000000 ) ) ;
#1220 = VECTOR ( 'NONE', #2563, 1000.000000000000000 ) ;
#1221 = CIRCLE ( 'NONE', #6857, 25.00000000000000000 ) ;
#1222 = VECTOR ( 'NONE', #6548, 1000.000000000000000 ) ;
#1223 = ORIENTED_EDGE ( 'NONE', *, *, #1408, .F. ) ;
#1224 = CIRCLE ( 'NONE', #5713, 12.49999999999999467 ) ;
#1225 = EDGE_LOOP ( 'NONE', ( #1493, #5646 ) ) ;
#1226 = EDGE_CURVE ( 'NONE', #5786, #28, #40, .T. ) ;
#1227 = DIRECTION ( 'NONE',  ( -1.000000000000000000, 0.000000000000000000, 0.000000000000000000 ) ) ;
#1228 = LINE ( 'NONE', #5600, #1125 ) ;
#1229 = FACE_OUTER_BOUND ( 'NONE', #1450, .T. ) ;
#1230 = DIRECTION ( 'NONE',  ( 0.8660254037844384856, 0.5000000000000003331, -0.000000000000000000 ) ) ;
#1231 = ORIENTED_EDGE ( 'NONE', *, *, #5161, .F. ) ;
#1232 = CARTESIAN_POINT ( 'NONE',  ( 158.9591979875528409, 23.33951095074252891, 25.00000000000000000 ) ) ;
#1233 = CIRCLE ( 'NONE', #2263, 12.50000000000000000 ) ;
#1234 = VERTEX_POINT ( 'NONE', #2416 ) ;
#1235 = CARTESIAN_POINT ( 'NONE',  ( 369.3855057752896300, 16.57606561041850313, 11.19744344920339962 ) ) ;
#1236 = ORIENTED_EDGE ( 'NONE', *, *, #7150, .T. ) ;
#1237 = CARTESIAN_POINT ( 'NONE',  ( 370.5191279495746244, -16.23886410922228052, 11.67632056536055707 ) ) ;
#1238 = CIRCLE ( 'NONE', #7509, 25.00000000000000000 ) ;
#1239 = EDGE_LOOP ( 'NONE', ( #7845, #1236, #3933, #3292 ) ) ;
#1240 = FILL_AREA_STYLE_COLOUR ( '', #96 ) ;
#1241 = CARTESIAN_POINT ( 'NONE',  ( -25.00000000000000000, -25.00000000000000000, 50.00000000000000000 ) ) ;
#1242 = AXIS2_PLACEMENT_3D ( 'NONE', #1410, #4297, #6871 ) ;
#1243 = ORIENTED_EDGE ( 'NONE', *, *, #3526, .F. ) ;
#1244 = ORIENTED_EDGE ( 'NONE', *, *, #5410, .F. ) ;
#1245 = ORIENTED_EDGE ( 'NONE', *, *, #6404, .F. ) ;
#1246 = DIRECTION ( 'NONE',  ( 1.000000000000000000, 0.000000000000000000, 0.000000000000000000 ) ) ;
#1247 = CARTESIAN_POINT ( 'NONE',  ( 387.4981577384509706, -19.99884858813039301, -0.8730781214943976742 ) ) ;
#1248 = CARTESIAN_POINT ( 'NONE',  ( 325.0000000000000000, 0.000000000000000000, 0.000000000000000000 ) ) ;
#1250 = CARTESIAN_POINT ( 'NONE',  ( 339.1025403784438481, 150.0000000000000568, 125.0000000000000000 ) ) ;
#1249 = VECTOR ( 'NONE', #3179, 1000.000000000000000 ) ;
#1251 = FACE_OUTER_BOUND ( 'NONE', #955, .T. ) ;
#1252 = ADVANCED_FACE ( 'NONE', ( #5586 ), #6106, .F. ) ;
#1253 = VECTOR ( 'NONE', #2042, 1000.000000000000000 ) ;
#1254 = EDGE_CURVE ( 'NONE', #1108, #3864, #3024, .T. ) ;
#1255 = DIRECTION ( 'NONE',  ( 1.000000000000000000, 0.000000000000000000, 0.000000000000000000 ) ) ;
#1256 = APPLICATION_PROTOCOL_DEFINITION ( 'draft international standard', 'automotive_design', 1998, #6182 ) ;
#1257 = FACE_BOUND ( 'NONE', #7583, .T. ) ;
#1258 = CARTESIAN_POINT ( 'NONE',  ( 326.6025403784438481, 142.5000000000000000, 125.0000000000000000 ) ) ;
#1259 = CARTESIAN_POINT ( 'NONE',  ( -37.49999999999965183, -4.857225732735003066E-14, 0.000000000000000000 ) ) ;
#1260 = FACE_BOUND ( 'NONE', #2868, .T. ) ;
#1261 = VECTOR ( 'NONE', #1281, 1000.000000000000000 ) ;
#1262 = AXIS2_PLACEMENT_3D ( 'NONE', #1379, #1861, #6122 ) ;
#1263 = EDGE_CURVE ( 'NONE', #2186, #7887, #7, .T. ) ;
#1264 = ORIENTED_EDGE ( 'NONE', *, *, #1299, .F. ) ;
#1265 = AXIS2_PLACEMENT_3D ( 'NONE', #7035, #929, #258 ) ;
#1266 = VECTOR ( 'NONE', #4939, 1000.000000000000000 ) ;
#1267 = ORIENTED_EDGE ( 'NONE', *, *, #4218, .T. ) ;
#1268 = DIRECTION ( 'NONE',  ( -1.000000000000000000, -0.000000000000000000, -0.000000000000000000 ) ) ;
#1269 = DIRECTION ( 'NONE',  ( 0.000000000000000000, 0.000000000000000000, 1.000000000000000000 ) ) ;
#1270 = DIRECTION ( 'NONE',  ( -0.7070068166729618353, -0.7072067315700302226, 0.000000000000000000 ) ) ;
#1271 =( LENGTH_UNIT ( ) NAMED_UNIT ( * ) SI_UNIT ( .MILLI., .METRE. ) );
#1272 = ORIENTED_EDGE ( 'NONE', *, *, #6816, .F. ) ;
#1273 = CARTESIAN_POINT ( 'NONE',  ( 0.000000000000000000, -25.00000000000000000, 25.00000000000000000 ) ) ;
#1274 = CIRCLE ( 'NONE', #5757, 5.000000000000000888 ) ;
#1275 = ORIENTED_EDGE ( 'NONE', *, *, #1932, .T. ) ;
#1276 = B_SPLINE_CURVE_WITH_KNOTS ( 'NONE', 3,
 ( #7605, #4554, #7009, #5806 ),
 .UNSPECIFIED., .F., .F.,
 ( 4, 4 ),
 ( 0.000000000000000000, 0.001270006434949985923 ),
 .UNSPECIFIED. ) ;
#1277 = CARTESIAN_POINT ( 'NONE',  ( 373.3129592716863385, 15.69785030319133945, 12.39275847443047773 ) ) ;
#1278 = ORIENTED_EDGE ( 'NONE', *, *, #900, .T. ) ;
#1279 = CARTESIAN_POINT ( 'NONE',  ( 368.6712260976869970, -16.83573837738345702, -10.80867071580873784 ) ) ;
#1280 = ORIENTED_EDGE ( 'NONE', *, *, #4577, .T. ) ;
#1281 = DIRECTION ( 'NONE',  ( -0.000000000000000000, -0.000000000000000000, -1.000000000000000000 ) ) ;
#1282 = CARTESIAN_POINT ( 'NONE',  ( 296.6025403784439050, 90.00000000000001421, 0.000000000000000000 ) ) ;
#1283 = EDGE_CURVE ( 'NONE', #4754, #2601, #75, .T. ) ;
#1284 = ORIENTED_EDGE ( 'NONE', *, *, #545, .T. ) ;
#1285 = ORIENTED_EDGE ( 'NONE', *, *, #2144, .F. ) ;
#1286 = ORIENTED_EDGE ( 'NONE', *, *, #6593, .T. ) ;
#1287 = DIRECTION ( 'NONE',  ( 1.000000000000000000, 0.000000000000000000, -0.000000000000000000 ) ) ;
#1288 = CARTESIAN_POINT ( 'NONE',  ( -27.49999999999989342, 187.4999999999999432, 0.000000000000000000 ) ) ;
#1289 = DIRECTION ( 'NONE',  ( 0.000000000000000000, -0.000000000000000000, 1.000000000000000000 ) ) ;
#1290 = DIRECTION ( 'NONE',  ( -1.000000000000000000, -0.000000000000000000, -0.000000000000000000 ) ) ;
#1291 = CARTESIAN_POINT ( 'NONE',  ( -17.50000000000000355, 0.000000000000000000, 77.49999999999998579 ) ) ;
#1292 = ITEM_DEFINED_TRANSFORMATION ( 'NONE', 'NONE', #6424,  #5785 ) ;
#1293 =( GEOMETRIC_REPRESENTATION_CONTEXT ( 3 ) GLOBAL_UNCERTAINTY_ASSIGNED_CONTEXT ( ( #6402 ) ) GLOBAL_UNIT_ASSIGNED_CONTEXT ( ( #2786, #5675, #4615 ) ) REPRESENTATION_CONTEXT ( 'NONE', 'WORKASPACE' ) );
#1294 = PRODUCT_DEFINITION ( 'UNKNOWN', '', #4114, #7124 ) ;
#1295 = DIRECTION ( 'NONE',  ( 1.000000000000000000, 0.000000000000000000, 0.000000000000000000 ) ) ;
#1296 = DIRECTION ( 'NONE',  ( 0.000000000000000000, 0.000000000000000000, 1.000000000000000000 ) ) ;
#1297 = DIRECTION ( 'NONE',  ( -1.000000000000000000, -0.000000000000000000, -0.000000000000000000 ) ) ;
#1298 = PLANE ( 'NONE',  #4390 ) ;
#1299 = EDGE_CURVE ( 'NONE', #2585, #136, #3706, .T. ) ;
#1300 = VERTEX_POINT ( 'NONE', #6743 ) ;
#1301 =( NAMED_UNIT ( * ) PLANE_ANGLE_UNIT ( ) SI_UNIT ( $, .RADIAN. ) );
#1302 = VERTEX_POINT ( 'NONE', #1250 ) ;
#1303 = EDGE_CURVE ( 'NONE', #1635, #1401, #4900, .T. ) ;
#1304 = LINE ( 'NONE', #1937, #6489 ) ;
#1305 = CARTESIAN_POINT ( 'NONE',  ( 42.50000000000000000, 37.50000000000003553, 12.50000000000000000 ) ) ;
#1306 = LINE ( 'NONE', #6200, #6968 ) ;
#1307 = CARTESIAN_POINT ( 'NONE',  ( 12.50000000000000000, 0.000000000000000000, 1.000000000000028644 ) ) ;
#1308 = ORIENTED_EDGE ( 'NONE', *, *, #5793, .T. ) ;
#1309 = EDGE_CURVE ( 'NONE', #7297, #6889, #2084, .T. ) ;
#1310 = CARTESIAN_POINT ( 'NONE',  ( -37.49999999999992184, 111.9999999999999289, 130.0000000000000000 ) ) ;
#1311 = EDGE_CURVE ( 'NONE', #7344, #2724, #6336, .T. ) ;
#1312 = CARTESIAN_POINT ( 'NONE',  ( 369.3970366575052822, 16.57206429410149795, -11.20336317960804884 ) ) ;
#1313 = EDGE_LOOP ( 'NONE', ( #6943, #440, #6860, #4930 ) ) ;
#1314 = CARTESIAN_POINT ( 'NONE',  ( -12.50000000000000355, 1.836970198721030378E-15, 97.50000000000000000 ) ) ;
#1315 = EDGE_LOOP ( 'NONE', ( #1639, #6362, #7095, #4419 ) ) ;
#1316 =( NAMED_UNIT ( * ) SI_UNIT ( $, .STERADIAN. ) SOLID_ANGLE_UNIT ( ) );
#1317 = DIRECTION ( 'NONE',  ( 1.000000000000000000, 0.000000000000000000, 0.000000000000000000 ) ) ;
#1318 = ORIENTED_EDGE ( 'NONE', *, *, #491, .F. ) ;
#1319 = ORIENTED_EDGE ( 'NONE', *, *, #7432, .F. ) ;
#1320 = VERTEX_POINT ( 'NONE', #5817 ) ;
#1321 = LINE ( 'NONE', #7427, #6508 ) ;
#1322 = EDGE_CURVE ( 'NONE', #7589, #2527, #2739, .T. ) ;
#1323 = CARTESIAN_POINT ( 'NONE',  ( 386.1955684391606951, -19.21001202690979781, 5.620007094727602848 ) ) ;
#1324 = CARTESIAN_POINT ( 'NONE',  ( 42.50000000000000000, 47.50000000000003553, 12.65877081724072362 ) ) ;
#1325 = CYLINDRICAL_SURFACE ( 'NONE', #4517, 74.99999999999995737 ) ;
#1326 = CARTESIAN_POINT ( 'NONE',  ( 296.6025403784437913, 135.0000000000000000, 12.50000000000000000 ) ) ;
#1327 = VECTOR ( 'NONE', #1568, 1000.000000000000000 ) ;
#1328 = PRODUCT_CONTEXT ( 'NONE', #2748, 'mechanical' ) ;
#1329 = AXIS2_PLACEMENT_3D ( 'NONE', #4466, #3349, #1458 ) ;
#1330 = DIRECTION ( 'NONE',  ( -0.000000000000000000, 0.000000000000000000, 1.000000000000000000 ) ) ;
#1331 = CARTESIAN_POINT ( 'NONE',  ( 325.0000000000000000, -12.50000000000000000, -21.65063509461096558 ) ) ;
#1332 = DIRECTION ( 'NONE',  ( -0.000000000000000000, 0.000000000000000000, 1.000000000000000000 ) ) ;
#1333 = CARTESIAN_POINT ( 'NONE',  ( 0.7190441502950423169, -5.595828947448873159, 12.50000000000000000 ) ) ;
#1334 = AXIS2_PLACEMENT_3D ( 'NONE', #5899, #3637, #6500 ) ;
#1335 = AXIS2_PLACEMENT_3D ( 'NONE', #14, #5547, #7319 ) ;
#1336 = VERTEX_POINT ( 'NONE', #6298 ) ;
#1337 = EDGE_LOOP ( 'NONE', ( #1191, #7737, #5657, #5850, #2431, #2191, #3607 ) ) ;
#1338 = CARTESIAN_POINT ( 'NONE',  ( 0.000000000000000000, 0.000000000000000000, 0.000000000000000000 ) ) ;
#1339 = CARTESIAN_POINT ( 'NONE',  ( 375.0000000000000000, 25.00000000000000000, 12.50000000000000711 ) ) ;
#1341 = LINE ( 'NONE', #4422, #7355 ) ;
#1340 = VECTOR ( 'NONE', #2847, 1000.000000000000000 ) ;
#1342 = VECTOR ( 'NONE', #6596, 1000.000000000000000 ) ;
#1343 = DIRECTION ( 'NONE',  ( 0.000000000000000000, 1.481552359947913884E-16, -1.000000000000000000 ) ) ;
#1344 = ORIENTED_EDGE ( 'NONE', *, *, #480, .T. ) ;
#1345 = CARTESIAN_POINT ( 'NONE',  ( 0.000000000000000000, 0.000000000000000000, 12.50000000000000000 ) ) ;
#1346 = EDGE_CURVE ( 'NONE', #5638, #2838, #3248, .T. ) ;
#1347 = VECTOR ( 'NONE', #1173, 1000.000000000000000 ) ;
#1348 = ORIENTED_EDGE ( 'NONE', *, *, #2046, .F. ) ;
#1349 = EDGE_CURVE ( 'NONE', #781, #3736, #5424, .T. ) ;
#1350 = DIRECTION ( 'NONE',  ( 0.000000000000000000, 0.000000000000000000, -1.000000000000000000 ) ) ;
#1351 = ORIENTED_EDGE ( 'NONE', *, *, #395, .F. ) ;
#1352 = DIRECTION ( 'NONE',  ( -1.000000000000000000, 4.270088556250607616E-16, -0.000000000000000000 ) ) ;
#1353 = ORIENTED_EDGE ( 'NONE', *, *, #7079, .T. ) ;
#1354 = FACE_BOUND ( 'NONE', #119, .T. ) ;
#1355 = VECTOR ( 'NONE', #917, 1000.000000000000000 ) ;
#1356 = DIRECTION ( 'NONE',  ( 0.000000000000000000, 0.000000000000000000, 1.000000000000000000 ) ) ;
#1357 = ORIENTED_EDGE ( 'NONE', *, *, #6320, .F. ) ;
#1358=STYLED_ITEM('',(#7948),#4135);
#1359 = ORIENTED_EDGE ( 'NONE', *, *, #190, .T. ) ;
#1360 = EDGE_LOOP ( 'NONE', ( #4025, #2570, #7727, #6406, #2402, #2235, #3213, #914, #6734, #1030 ) ) ;
#1361 = CARTESIAN_POINT ( 'NONE',  ( 0.000000000000000000, 0.000000000000000000, 0.5000000000000004441 ) ) ;
#1362 = CARTESIAN_POINT ( 'NONE',  ( 6.249999999999977796, 0.000000000000000000, 25.00000000000000000 ) ) ;
#1363 = CARTESIAN_POINT ( 'NONE',  ( 75.00000000000000000, 10.56842436860067735, 25.00000000000000000 ) ) ;
#1364 = EDGE_LOOP ( 'NONE', ( #1805, #6622, #438, #7201, #5845 ) ) ;
#1365 = FACE_OUTER_BOUND ( 'NONE', #3266, .T. ) ;
#1366 = CIRCLE ( 'NONE', #3932, 12.50000000000001066 ) ;
#1367 = EDGE_CURVE ( 'NONE', #6805, #2766, #3369, .T. ) ;
#1368 = VECTOR ( 'NONE', #6947, 1000.000000000000000 ) ;
#1369 = DIRECTION ( 'NONE',  ( -1.000000000000000000, 0.000000000000000000, -0.000000000000000000 ) ) ;
#1370 = DIRECTION ( 'NONE',  ( 0.000000000000000000, -1.000000000000000000, 0.000000000000000000 ) ) ;
#1371 = CARTESIAN_POINT ( 'NONE',  ( -36.78095584970496645, 12.70544120911856290, 12.50000000000000000 ) ) ;
#1372 = CARTESIAN_POINT ( 'NONE',  ( 0.000000000000000000, 0.000000000000000000, 0.000000000000000000 ) ) ;
#1373 = CIRCLE ( 'NONE', #6763, 5.000000000000004441 ) ;
#1374 = EDGE_CURVE ( 'NONE', #2940, #4850, #360, .T. ) ;
#1375 = ORIENTED_EDGE ( 'NONE', *, *, #3903, .F. ) ;
#1376 = DIRECTION ( 'NONE',  ( 0.7071067811865517916, 0.000000000000000000, -0.7071067811865431318 ) ) ;
#1377 = VERTEX_POINT ( 'NONE', #797 ) ;
#1378 = CIRCLE ( 'NONE', #1786, 24.99999996734539920 ) ;
#1379 = CARTESIAN_POINT ( 'NONE',  ( 62.50000000000008527, 111.9999999999998863, 130.0000000000000000 ) ) ;
#1380 = FACE_OUTER_BOUND ( 'NONE', #1581, .T. ) ;
#1381 = CARTESIAN_POINT ( 'NONE',  ( -8.959197987552832032, 23.33951095074251114, 25.00000000000000000 ) ) ;
#1382 = VERTEX_POINT ( 'NONE', #7021 ) ;
#1383 = MANIFOLD_SOLID_BREP ( 'Pah2', #6579 ) ;
#1384 = CARTESIAN_POINT ( 'NONE',  ( 0.7190441502950353225, 62.70544120911855401, 12.50000000000000000 ) ) ;
#1385 = AXIS2_PLACEMENT_3D ( 'NONE', #2830, #5264, #5389 ) ;
#1386 = VERTEX_POINT ( 'NONE', #199 ) ;
#1387 = CARTESIAN_POINT ( 'NONE',  ( 365.1198422076048473, 18.47484582708395706, -7.667708004838452496 ) ) ;
#1388 = ORIENTED_EDGE ( 'NONE', *, *, #7148, .F. ) ;
#1389 = DIRECTION ( 'NONE',  ( -1.000000000000000000, 0.000000000000000000, 0.000000000000000000 ) ) ;
#1390 = VERTEX_POINT ( 'NONE', #5157 ) ;
#1391 = ADVANCED_FACE ( 'NONE', ( #2650 ), #6375, .F. ) ;
#1392 = CYLINDRICAL_SURFACE ( 'NONE', #2147, 32.75000000000001421 ) ;
#1393 = AXIS2_PLACEMENT_3D ( 'NONE', #5095, #7550, #3299 ) ;
#1394 = CARTESIAN_POINT ( 'NONE',  ( 200.0000000000000000, -37.50000000000000711, 12.50000000000000000 ) ) ;
#1395 = ADVANCED_FACE ( 'NONE', ( #2043 ), #4916, .T. ) ;
#1396 = VERTEX_POINT ( 'NONE', #2691 ) ;
#1397 = AXIS2_PLACEMENT_3D ( 'NONE', #5187, #2105, #6927 ) ;
#1398 = CARTESIAN_POINT ( 'NONE',  ( 398.6828372460798846, -12.50000000000000000, 14.73776325548316812 ) ) ;
#1399 = VERTEX_POINT ( 'NONE', #2770 ) ;
#1400 = EDGE_CURVE ( 'NONE', #530, #3850, #5781, .T. ) ;
#1401 = VERTEX_POINT ( 'NONE', #2166 ) ;
#1402 = DIRECTION ( 'NONE',  ( -0.4463453945640545317, -2.137850715617611764E-16, 0.8948607650084221543 ) ) ;
#1403 = ADVANCED_FACE ( 'NONE', ( #2855 ), #4310, .F. ) ;
#1404 = CARTESIAN_POINT ( 'NONE',  ( 386.8066430167523890, -19.57388548866421019, -4.126530372600788255 ) ) ;
#1405 = CARTESIAN_POINT ( 'NONE',  ( 375.0000000000000000, 12.50000000000000000, 3.061616997868383043E-15 ) ) ;
#1406 = ORIENTED_EDGE ( 'NONE', *, *, #7332, .T. ) ;
#1407 = PLANE ( 'NONE',  #4149 ) ;
#1408 = EDGE_CURVE ( 'NONE', #4601, #6800, #2511, .T. ) ;
#1409 = EDGE_CURVE ( 'NONE', #4343, #994, #1151, .T. ) ;
#1410 = CARTESIAN_POINT ( 'NONE',  ( 350.0000000000001137, -6.123233995736758985E-15, 25.00000000000000000 ) ) ;
#1411 = FACE_OUTER_BOUND ( 'NONE', #3002, .T. ) ;
#1412 = CARTESIAN_POINT ( 'NONE',  ( 400.0000000000000568, 0.000000000000000000, 25.00000000000000000 ) ) ;
#1413 = DIRECTION ( 'NONE',  ( -1.000000000000000000, 0.000000000000000000, 0.000000000000000000 ) ) ;
#1414 = EDGE_LOOP ( 'NONE', ( #5458, #2479, #1627, #1182 ) ) ;
#1415 = CARTESIAN_POINT ( 'NONE',  ( 13.21904415029503355, 62.70544120911855401, 12.50000000000000000 ) ) ;
#1416 = ORIENTED_EDGE ( 'NONE', *, *, #5665, .T. ) ;
#1417 = FACE_OUTER_BOUND ( 'NONE', #4360, .T. ) ;
#1418 = CARTESIAN_POINT ( 'NONE',  ( 0.000000000000000000, -25.00000000000000000, 0.000000000000000000 ) ) ;
#1419 = CARTESIAN_POINT ( 'NONE',  ( 0.000000000000000000, 0.000000000000000000, 75.00000000000000000 ) ) ;
#1420 = EDGE_CURVE ( 'NONE', #3234, #1820, #7369, .T. ) ;
#1421 = CARTESIAN_POINT ( 'NONE',  ( -25.00000000000000000, 0.000000000000000000, -12.50000000000000000 ) ) ;
#1422 = ORIENTED_EDGE ( 'NONE', *, *, #5037, .F. ) ;
#1423 = ORIENTED_EDGE ( 'NONE', *, *, #666, .F. ) ;
#1424 = DIRECTION ( 'NONE',  ( 1.000000000000000000, 0.000000000000000000, 0.000000000000000000 ) ) ;
#1425 = ORIENTED_EDGE ( 'NONE', *, *, #2926, .F. ) ;
#1426 = CARTESIAN_POINT ( 'NONE',  ( -15.64999999999999680, 0.000000000000000000, 49.99999999999998579 ) ) ;
#1427 = ORIENTED_EDGE ( 'NONE', *, *, #3585, .F. ) ;
#1428 = CARTESIAN_POINT ( 'NONE',  ( 52.50000000000000711, 0.000000000000000000, 12.50000000000000000 ) ) ;
#1429 = DIRECTION ( 'NONE',  ( 1.000000000000000000, 0.000000000000000000, 0.000000000000000000 ) ) ;
#1430 = ORIENTED_EDGE ( 'NONE', *, *, #6604, .T. ) ;
#1431 = CARTESIAN_POINT ( 'NONE',  ( 0.000000000000000000, 0.000000000000000000, 47.50000000000000000 ) ) ;
#1432 = EDGE_LOOP ( 'NONE', ( #837, #5779, #6835 ) ) ;
#1433 = ORIENTED_EDGE ( 'NONE', *, *, #1011, .F. ) ;
#1434 = ADVANCED_BREP_SHAPE_REPRESENTATION ( '', ( #4135, #5785 ), #2447 ) ;
#1435 = DIRECTION ( 'NONE',  ( -1.000000000000000000, 1.224646799147353454E-16, 0.000000000000000000 ) ) ;
#1436 = CARTESIAN_POINT ( 'NONE',  ( -6.495190528383286477, 16.25000000000000000, 7.500000000000000000 ) ) ;
#1437 = CARTESIAN_POINT ( 'NONE',  ( 400.0000000000000000, 12.50000000000000000, -12.95183384698871620 ) ) ;
#1438 = ORIENTED_EDGE ( 'NONE', *, *, #6023, .F. ) ;
#1439 = LINE ( 'NONE', #5290, #447 ) ;
#1440 = ADVANCED_FACE ( 'NONE', ( #1864 ), #5483, .F. ) ;
#1441 = ADVANCED_FACE ( 'NONE', ( #7880, #1641 ), #6164, .F. ) ;
#1442 = CONTEXT_DEPENDENT_SHAPE_REPRESENTATION ( #4180, #1881 ) ;
#1443 = CARTESIAN_POINT ( 'NONE',  ( -11.64999999999996660, 0.000000000000000000, 200.0000000000000000 ) ) ;
#1444 = CARTESIAN_POINT ( 'NONE',  ( 0.000000000000000000, 25.00000000000000000, 0.000000000000000000 ) ) ;
#1445 = CARTESIAN_POINT ( 'NONE',  ( 0.000000000000000000, 87.70544117646394966, 12.50000000000000000 ) ) ;
#1446 = AXIS2_PLACEMENT_3D ( 'NONE', #2679, #5114, #7568 ) ;
#1447 = DIRECTION ( 'NONE',  ( -1.000000000000000000, -0.000000000000000000, -0.000000000000000000 ) ) ;
#1448 = EDGE_CURVE ( 'NONE', #2355, #1785, #7368, .T. ) ;
#1449 = EDGE_CURVE ( 'NONE', #3005, #5496, #696, .T. ) ;
#1450 = EDGE_LOOP ( 'NONE', ( #5658, #6096, #3235, #1646 ) ) ;
#1451 = CIRCLE ( 'NONE', #6077, 5.000000000000004441 ) ;
#1452 = AXIS2_PLACEMENT_3D ( 'NONE', #5182, #2789, #7518 ) ;
#1453 = DIRECTION ( 'NONE',  ( 0.000000000000000000, 0.000000000000000000, 1.000000000000000000 ) ) ;
#1454 = CARTESIAN_POINT ( 'NONE',  ( 332.3707862481380744, 209.6990734970208621, 245.6227876318357914 ) ) ;
#1455 = ORIENTED_EDGE ( 'NONE', *, *, #7150, .F. ) ;
#1456 = SURFACE_STYLE_USAGE ( .BOTH. , #6277 ) ;
#1457 = DIRECTION ( 'NONE',  ( 1.000000000000000000, 0.000000000000000000, 0.000000000000000000 ) ) ;
#1458 = DIRECTION ( 'NONE',  ( 1.000000000000000000, 0.000000000000000000, -0.000000000000000000 ) ) ;
#1459 = DIRECTION ( 'NONE',  ( 0.000000000000000000, 0.000000000000000000, -1.000000000000000000 ) ) ;
#1460 = ORIENTED_EDGE ( 'NONE', *, *, #4730, .F. ) ;
#1461 = AXIS2_PLACEMENT_3D ( 'NONE', #800, #4329, #3748 ) ;
#1462 = AXIS2_PLACEMENT_3D ( 'NONE', #3077, #5511, #7908 ) ;
#1463 = ORIENTED_EDGE ( 'NONE', *, *, #2340, .T. ) ;
#1464 = EDGE_CURVE ( 'NONE', #4603, #2527, #3042, .T. ) ;
#1465 = VECTOR ( 'NONE', #643, 1000.000000000000000 ) ;
#1466 = DIRECTION ( 'NONE',  ( -1.000000000000000000, 0.000000000000000000, 0.000000000000000000 ) ) ;
#1467 = AXIS2_PLACEMENT_3D ( 'NONE', #6840, #4467, #1459 ) ;
#1468 = ORIENTED_EDGE ( 'NONE', *, *, #6355, .T. ) ;
#1469 = AXIS2_PLACEMENT_3D ( 'NONE', #5254, #1128, #3421 ) ;
#1470 = FACE_OUTER_BOUND ( 'NONE', #5331, .T. ) ;
#1471 = CARTESIAN_POINT ( 'NONE',  ( 286.6025403784437913, 150.0000000000000284, 12.50000000000000000 ) ) ;
#1472 = CARTESIAN_POINT ( 'NONE',  ( -25.00000000000000000, 0.000000000000000000, 0.000000000000000000 ) ) ;
#1473 = DIRECTION ( 'NONE',  ( -1.000000000000000000, 3.469446951953614189E-17, 0.000000000000000000 ) ) ;
#1474 = CIRCLE ( 'NONE', #4544, 24.99999996734539920 ) ;
#1475 = MANIFOLD_SOLID_BREP ( 'Radyus2', #6708 ) ;
#1476 = ORIENTED_EDGE ( 'NONE', *, *, #4050, .F. ) ;
#1477 = VERTEX_POINT ( 'NONE', #2436 ) ;
#1478 = CIRCLE ( 'NONE', #6101, 12.50000000000001066 ) ;
#1479 = ORIENTED_EDGE ( 'NONE', *, *, #997, .T. ) ;
#1480 = CARTESIAN_POINT ( 'NONE',  ( -13.00000000000000178, 1.592040838891559293E-15, 6.999999999999999112 ) ) ;
#1481 = CARTESIAN_POINT ( 'NONE',  ( 0.000000000000000000, 0.000000000000000000, 45.00000000000000000 ) ) ;
#1482 = FACE_BOUND ( 'NONE', #7374, .T. ) ;
#1483 = AXIS2_PLACEMENT_3D ( 'NONE', #3399, #3956, #5924 ) ;
#1484 = ORIENTED_EDGE ( 'NONE', *, *, #6553, .T. ) ;
#1485 = PRODUCT_DEFINITION_SHAPE ( 'NONE', 'NONE',  #7918 ) ;
#1486 = DIRECTION ( 'NONE',  ( -0.000000000000000000, -0.000000000000000000, 1.000000000000000000 ) ) ;
#1487 = DIRECTION ( 'NONE',  ( 1.000000000000000000, 1.261617073437677999E-16, 0.000000000000000000 ) ) ;
#1489 = CARTESIAN_POINT ( 'NONE',  ( 325.0000000000000000, 12.50000000000000000, -21.65063509461096913 ) ) ;
#1488 = CIRCLE ( 'NONE', #6749, 25.00000000000000000 ) ;
#1490 = DIRECTION ( 'NONE',  ( -1.000000000000000000, 0.000000000000000000, 0.000000000000000000 ) ) ;
#1491 = EDGE_CURVE ( 'NONE', #6485, #7566, #4024, .T. ) ;
#1492 = ADVANCED_FACE ( 'NONE', ( #7328 ), #1824, .F. ) ;
#1493 = ORIENTED_EDGE ( 'NONE', *, *, #4826, .T. ) ;
#1494 = CIRCLE ( 'NONE', #348, 11.49999999999995914 ) ;
#1495 = DIRECTION ( 'NONE',  ( 1.000000000000000000, 0.000000000000000000, 0.000000000000000000 ) ) ;
#1496 = CARTESIAN_POINT ( 'NONE',  ( -17.31851962845015791, 164.1990734970206063, 183.2402661832476554 ) ) ;
#1497 = VERTEX_POINT ( 'NONE', #6125 ) ;
#1498 = CARTESIAN_POINT ( 'NONE',  ( 17.50000000000000355, 2.143131898507868643E-15, 90.00000000000000000 ) ) ;
#1499 = CARTESIAN_POINT ( 'NONE',  ( 400.0000000000000000, -12.50000000000000000, 12.95183384698871620 ) ) ;
#1500 = CARTESIAN_POINT ( 'NONE',  ( 12.50000000000000000, 1.530808498934191521E-15, 75.00000000000000000 ) ) ;
#1501 = EDGE_CURVE ( 'NONE', #1166, #1399, #2753, .T. ) ;
#1502 = DIRECTION ( 'NONE',  ( -0.000000000000000000, 0.000000000000000000, 1.000000000000000000 ) ) ;
#1503 = ORIENTED_EDGE ( 'NONE', *, *, #4873, .T. ) ;
#1504 = EDGE_CURVE ( 'NONE', #3922, #3451, #4925, .T. ) ;
#1505 = CIRCLE ( 'NONE', #4956, 25.00000000000000000 ) ;
#1506 = UNCERTAINTY_MEASURE_WITH_UNIT (LENGTH_MEASURE( 1.000000000000000082E-05 ), #4897, 'distance_accuracy_value', 'NONE');
#1507 = VERTEX_POINT ( 'NONE', #3834 ) ;
#1508 = VECTOR ( 'NONE', #3531, 1000.000000000000000 ) ;
#1509 = VECTOR ( 'NONE', #6262, 1000.000000000000000 ) ;
#1510 = DIRECTION ( 'NONE',  ( -0.000000000000000000, -1.000000000000000000, -0.000000000000000000 ) ) ;
#1511 = ORIENTED_EDGE ( 'NONE', *, *, #1400, .F. ) ;
#1512 = DIRECTION ( 'NONE',  ( 0.000000000000000000, 0.000000000000000000, -1.000000000000000000 ) ) ;
#1513 = CYLINDRICAL_SURFACE ( 'NONE', #7735, 17.50000000000000355 ) ;
#1514 = CARTESIAN_POINT ( 'NONE',  ( -26.24999999999997158, 47.34122918275937053, 12.50000000000000000 ) ) ;
#1515 = AXIS2_PLACEMENT_3D ( 'NONE', #3832, #6278, #20 ) ;
#1516 = APPLICATION_CONTEXT ( 'automotive_design' ) ;
#1517 = ORIENTED_EDGE ( 'NONE', *, *, #291, .T. ) ;
#1518 = CARTESIAN_POINT ( 'NONE',  ( 0.000000000000000000, 0.000000000000000000, 52.50000000000000000 ) ) ;
#1519 = VERTEX_POINT ( 'NONE', #7561 ) ;
#1520 = AXIS2_PLACEMENT_3D ( 'NONE', #3586, #3710, #1775 ) ;
#1521 = CARTESIAN_POINT ( 'NONE',  ( 0.000000000000000000, 0.000000000000000000, 0.000000000000000000 ) ) ;
#1522 = AXIS2_PLACEMENT_3D ( 'NONE', #164, #207, #2050 ) ;
#1523 = ORIENTED_EDGE ( 'NONE', *, *, #7264, .F. ) ;
#1524 = DIRECTION ( 'NONE',  ( 0.000000000000000000, 0.000000000000000000, 1.000000000000000000 ) ) ;
#1525 = CARTESIAN_POINT ( 'NONE',  ( 50.71904415029504065, 62.70544120911855401, 0.000000000000000000 ) ) ;
#1526 = PLANE ( 'NONE',  #4963 ) ;
#1527 = DIRECTION ( 'NONE',  ( -1.000000000000000000, 0.000000000000000000, 0.000000000000000000 ) ) ;
#1528 = EDGE_CURVE ( 'NONE', #3115, #3875, #3910, .T. ) ;
#1529 = AXIS2_PLACEMENT_3D ( 'NONE', #2288, #1796, #1678 ) ;
#1530 = CIRCLE ( 'NONE', #4722, 4.999999999999997335 ) ;
#1531 = ORIENTED_EDGE ( 'NONE', *, *, #385, .F. ) ;
#1532 = DIRECTION ( 'NONE',  ( 1.000000000000000000, 0.000000000000000000, 0.000000000000000000 ) ) ;
#1533 = DIRECTION ( 'NONE',  ( 0.000000000000000000, 0.000000000000000000, 1.000000000000000000 ) ) ;
#1534 = CARTESIAN_POINT ( 'NONE',  ( 0.000000000000000000, -5.595828947448873159, 12.50000000000000000 ) ) ;
#1535 = LINE ( 'NONE', #6428, #7102 ) ;
#1536 = DIRECTION ( 'NONE',  ( -0.000000000000000000, -1.000000000000000000, -0.000000000000000000 ) ) ;
#1537 = CARTESIAN_POINT ( 'NONE',  ( 158.9591979875528409, 23.33951095074252891, 25.00000000000000000 ) ) ;
#1538 = PRODUCT_DEFINITION ( 'UNKNOWN', '', #6554, #3353 ) ;
#1539 = ORIENTED_EDGE ( 'NONE', *, *, #68, .F. ) ;
#1540 = DIRECTION ( 'NONE',  ( -0.5000000000000004441, -0.8660254037844383745, 0.000000000000000000 ) ) ;
#1541 = CARTESIAN_POINT ( 'NONE',  ( -37.50000000000000000, 4.857225732735047243E-14, 12.50000000000000000 ) ) ;
#1542 = PLANE ( 'NONE',  #45 ) ;
#1543 =( LENGTH_UNIT ( ) NAMED_UNIT ( * ) SI_UNIT ( .MILLI., .METRE. ) );
#1544 = VERTEX_POINT ( 'NONE', #264 ) ;
#1545 = EDGE_CURVE ( 'NONE', #3479, #7501, #3761, .T. ) ;
#1546 = DIRECTION ( 'NONE',  ( -0.000000000000000000, -0.000000000000000000, -1.000000000000000000 ) ) ;
#1547 = VERTEX_POINT ( 'NONE', #780 ) ;
#1548 = CARTESIAN_POINT ( 'NONE',  ( 375.0000000000000000, 25.00000000000000000, 3.061616997868383043E-15 ) ) ;
#1549 = DIRECTION ( 'NONE',  ( 1.000000000000000000, -4.789677997474686366E-16, 0.000000000000000000 ) ) ;
#1550 = ADVANCED_FACE ( 'NONE', ( #2708 ), #6924, .T. ) ;
#1551 = DIRECTION ( 'NONE',  ( 0.000000000000000000, -0.000000000000000000, -1.000000000000000000 ) ) ;
#1552 = DIRECTION ( 'NONE',  ( -0.000000000000000000, -0.000000000000000000, -1.000000000000000000 ) ) ;
#1553 = EDGE_CURVE ( 'NONE', #819, #7797, #4539, .T. ) ;
#1554 = VERTEX_POINT ( 'NONE', #4348 ) ;
#1555 = LINE ( 'NONE', #2850, #5881 ) ;
#1556 = ORIENTED_EDGE ( 'NONE', *, *, #4165, .T. ) ;
#1557 = DIRECTION ( 'NONE',  ( 1.000000000000000000, 0.000000000000000000, 0.000000000000000000 ) ) ;
#1558 = ORIENTED_EDGE ( 'NONE', *, *, #5495, .T. ) ;
#1559 = DIRECTION ( 'NONE',  ( -0.000000000000000000, -0.000000000000000000, -1.000000000000000000 ) ) ;
#1560 = DIRECTION ( 'NONE',  ( 1.000000000000000000, 0.000000000000000000, 0.000000000000000000 ) ) ;
#1561 = DIRECTION ( 'NONE',  ( -0.000000000000000000, 0.000000000000000000, 1.000000000000000000 ) ) ;
#1562 = DIRECTION ( 'NONE',  ( -1.000000000000000000, 0.000000000000000000, 0.000000000000000000 ) ) ;
#1563 = VERTEX_POINT ( 'NONE', #4996 ) ;
#1564 = ADVANCED_FACE ( 'NONE', ( #102 ), #5680, .T. ) ;
#1565 = DIRECTION ( 'NONE',  ( 0.000000000000000000, -0.000000000000000000, 1.000000000000000000 ) ) ;
#1566 = LINE ( 'NONE', #5710, #7424 ) ;
#1567 = DIRECTION ( 'NONE',  ( 1.000000000000000000, -0.000000000000000000, -0.000000000000000000 ) ) ;
#1568 = DIRECTION ( 'NONE',  ( -1.000000000000000000, 4.270088556250607616E-16, -0.000000000000000000 ) ) ;
#1569 = CARTESIAN_POINT ( 'NONE',  ( 385.1211727163475302, 18.60519396204907139, 7.346513279853128964 ) ) ;
#1570 = DIRECTION ( 'NONE',  ( -1.000000000000000000, 0.000000000000000000, 0.000000000000000000 ) ) ;
#1571 = DIRECTION ( 'NONE',  ( 4.789593822244094799E-16, 1.000000000000000000, 5.328524654824031087E-22 ) ) ;
#1572 = ORIENTED_EDGE ( 'NONE', *, *, #2376, .T. ) ;
#1573 = CARTESIAN_POINT ( 'NONE',  ( 375.0000000000000000, -12.50000000000000355, 3.061616997868383043E-15 ) ) ;
#1574 = CARTESIAN_POINT ( 'NONE',  ( 0.000000000000000000, 0.000000000000000000, 200.0000000000000000 ) ) ;
#1575 = LINE ( 'NONE', #3949, #4277 ) ;
#1576 = ORIENTED_EDGE ( 'NONE', *, *, #4704, .F. ) ;
#1577 = AXIS2_PLACEMENT_3D ( 'NONE', #5427, #7870, #4821 ) ;
#1578 = VERTEX_POINT ( 'NONE', #4508 ) ;
#1579 = ORIENTED_EDGE ( 'NONE', *, *, #5495, .F. ) ;
#1580 = CARTESIAN_POINT ( 'NONE',  ( 25.71904415029483459, 19.40417101989674009, 0.000000000000000000 ) ) ;
#1581 = EDGE_LOOP ( 'NONE', ( #940, #7168, #1751, #4070 ) ) ;
#1582 = DIRECTION ( 'NONE',  ( 1.000000000000000000, -4.270088556250607616E-16, 0.000000000000000000 ) ) ;
#1583 = VERTEX_POINT ( 'NONE', #6356 ) ;
#1584 = CIRCLE ( 'NONE', #4015, 13.00000000000000178 ) ;
#1585 = ORIENTED_EDGE ( 'NONE', *, *, #7514, .T. ) ;
#1586 = CARTESIAN_POINT ( 'NONE',  ( -12.50000000000000000, 0.000000000000000000, 75.00000000000000000 ) ) ;
#1587 = EDGE_CURVE ( 'NONE', #6561, #1, #5067, .T. ) ;
#1588 = CONICAL_SURFACE ( 'NONE', #1844, 12.50000000000000000, 0.7853981633974543852 ) ;
#1589 = EDGE_CURVE ( 'NONE', #7759, #7887, #6804, .T. ) ;
#1590 = COLOUR_RGB ( '',0.7921568627450980005, 0.8196078431372548767, 0.9333333333333333481 ) ;
#1591 = ORIENTED_EDGE ( 'NONE', *, *, #1163, .T. ) ;
#1592 = CIRCLE ( 'NONE', #1849, 9.999999999999896971 ) ;
#1593 = DIRECTION ( 'NONE',  ( 1.000000000000000000, 0.000000000000000000, 0.000000000000000000 ) ) ;
#1594 = EDGE_LOOP ( 'NONE', ( #7601, #815, #608, #1006 ) ) ;
#1595 = CARTESIAN_POINT ( 'NONE',  ( 326.6025403784438481, 217.5000000000000284, 125.0000000000000000 ) ) ;
#1596 = ORIENTED_EDGE ( 'NONE', *, *, #1018, .F. ) ;
#1597 = CARTESIAN_POINT ( 'NONE',  ( -12.50000000000000000, 0.000000000000000000, 0.000000000000000000 ) ) ;
#1598 = DIRECTION ( 'NONE',  ( 1.000000000000000000, 0.000000000000000000, 0.000000000000000000 ) ) ;
#1599 = AXIS2_PLACEMENT_3D ( 'NONE', #2483, #1356, #5654 ) ;
#1600 = EDGE_CURVE ( 'NONE', #2808, #243, #6882, .T. ) ;
#1601 = AXIS2_PLACEMENT_3D ( 'NONE', #2217, #972, #2132 ) ;
#1602 = AXIS2_PLACEMENT_3D ( 'NONE', #2780, #7665, #2174 ) ;
#1603 = DIRECTION ( 'NONE',  ( -0.000000000000000000, -0.000000000000000000, -1.000000000000000000 ) ) ;
#1604 = VECTOR ( 'NONE', #2925, 1000.000000000000000 ) ;
#1605 = ORIENTED_EDGE ( 'NONE', *, *, #2734, .T. ) ;
#1606 = LINE ( 'NONE', #4008, #1368 ) ;
#1607 = DIRECTION ( 'NONE',  ( -1.000000000000000000, 0.000000000000000000, 0.000000000000000000 ) ) ;
#1608 = DIRECTION ( 'NONE',  ( -0.000000000000000000, -0.000000000000000000, -1.000000000000000000 ) ) ;
#1609 = DIRECTION ( 'NONE',  ( -0.000000000000000000, -0.000000000000000000, -1.000000000000000000 ) ) ;
#1610 = CIRCLE ( 'NONE', #6227, 65.50000000000000000 ) ;
#1611 = DIRECTION ( 'NONE',  ( -0.000000000000000000, -0.000000000000000000, -1.000000000000000000 ) ) ;
#1612 = EDGE_CURVE ( 'NONE', #5578, #4376, #3391, .T. ) ;
#1613 = FACE_OUTER_BOUND ( 'NONE', #1315, .T. ) ;
#1614 = AXIS2_PLACEMENT_3D ( 'NONE', #5846, #7129, #1628 ) ;
#1615 = APPLICATION_PROTOCOL_DEFINITION ( 'draft international standard', 'automotive_design', 1998, #133 ) ;
#1616 = ORIENTED_EDGE ( 'NONE', *, *, #33, .F. ) ;
#1617 = DIRECTION ( 'NONE',  ( 0.3583679195021131081, -0.9335804380297002547, 0.000000000000000000 ) ) ;
#1618 = LINE ( 'NONE', #1178, #2300 ) ;
#1619 = PLANE ( 'NONE',  #822 ) ;
#1620 = VERTEX_POINT ( 'NONE', #6201 ) ;
#1621 = PRODUCT ( 'Sheet Metal Base', 'Sheet Metal Base', '', ( #6672 ) ) ;
#1622 = ADVANCED_FACE ( 'NONE', ( #3198 ), #5959, .T. ) ;
#1623 = VECTOR ( 'NONE', #7760, 1000.000000000000000 ) ;
#1624 = ORIENTED_EDGE ( 'NONE', *, *, #3027, .T. ) ;
#1625 = ORIENTED_EDGE ( 'NONE', *, *, #3090, .T. ) ;
#1626 =( NAMED_UNIT ( * ) PLANE_ANGLE_UNIT ( ) SI_UNIT ( $, .RADIAN. ) );
#1627 = ORIENTED_EDGE ( 'NONE', *, *, #5908, .T. ) ;
#1628 = DIRECTION ( 'NONE',  ( 1.000000000000000000, 0.000000000000000000, 0.000000000000000000 ) ) ;
#1629 = CIRCLE ( 'NONE', #222, 12.50000000000000000 ) ;
#1630 = CARTESIAN_POINT ( 'NONE',  ( -25.00000000000000000, -25.00000000000000000, 0.000000000000000000 ) ) ;
#1631 = ORIENTED_EDGE ( 'NONE', *, *, #911, .F. ) ;
#1632 = CARTESIAN_POINT ( 'NONE',  ( 42.50000000000000711, 182.5000000000000000, 12.50000000000000000 ) ) ;
#1633 = CARTESIAN_POINT ( 'NONE',  ( -25.00000000000000000, 0.000000000000000000, 0.000000000000000000 ) ) ;
#1634 = VECTOR ( 'NONE', #1559, 1000.000000000000000 ) ;
#1635 = VERTEX_POINT ( 'NONE', #744 ) ;
#1636 = DIRECTION ( 'NONE',  ( -0.4463453945640545317, 0.000000000000000000, 0.8948607650084221543 ) ) ;
#1637 = VERTEX_POINT ( 'NONE', #5602 ) ;
#1638 = DIRECTION ( 'NONE',  ( 1.000000000000000000, 0.000000000000000000, 0.000000000000000000 ) ) ;
#1639 = ORIENTED_EDGE ( 'NONE', *, *, #7090, .T. ) ;
#1640 = VECTOR ( 'NONE', #7186, 1000.000000000000000 ) ;
#1641 = FACE_OUTER_BOUND ( 'NONE', #3480, .T. ) ;
#1642 = DIRECTION ( 'NONE',  ( 1.000000000000000000, 0.000000000000000000, 0.000000000000000000 ) ) ;
#1643 = CIRCLE ( 'NONE', #6129, 12.50000000000000355 ) ;
#1644 = EDGE_CURVE ( 'NONE', #1399, #1166, #4532, .T. ) ;
#1645 = CARTESIAN_POINT ( 'NONE',  ( -12.99038105676657651, 1.734723475976807094E-15, 7.500000000000000000 ) ) ;
#1646 = ORIENTED_EDGE ( 'NONE', *, *, #7671, .F. ) ;
#1647 = AXIS2_PLACEMENT_3D ( 'NONE', #5772, #5115, #2598 ) ;
#1648 = AXIS2_PLACEMENT_3D ( 'NONE', #3340, #2737, #2011 ) ;
#1649 = EDGE_CURVE ( 'NONE', #6259, #1787, #5027, .T. ) ;
#1650 = ORIENTED_EDGE ( 'NONE', *, *, #4197, .F. ) ;
#1651 = EDGE_CURVE ( 'NONE', #7564, #4430, #4423, .T. ) ;
#1652 = FACE_OUTER_BOUND ( 'NONE', #7190, .T. ) ;
#1653 = CARTESIAN_POINT ( 'NONE',  ( 0.000000000000000000, 187.5000000000000000, 12.50000000000000000 ) ) ;
#1654 = EDGE_CURVE ( 'NONE', #7759, #3356, #7610, .T. ) ;
#1655 = DIRECTION ( 'NONE',  ( 0.000000000000000000, 0.000000000000000000, 1.000000000000000000 ) ) ;
#1656 = AXIS2_PLACEMENT_3D ( 'NONE', #2952, #1019, #5386 ) ;
#1657 = AXIS2_PLACEMENT_3D ( 'NONE', #5253, #1689, #5295 ) ;
#1658 = DIRECTION ( 'NONE',  ( -0.000000000000000000, 0.000000000000000000, 1.000000000000000000 ) ) ;
#1659 = ADVANCED_FACE ( 'NONE', ( #2916, #5307, #3388, #5183, #7043, #5879 ), #468, .T. ) ;
#1660 = CARTESIAN_POINT ( 'NONE',  ( 296.6025403784437913, 135.0000000000000000, 0.000000000000000000 ) ) ;
#1661 = SHAPE_DEFINITION_REPRESENTATION ( #6491, #6910 ) ;
#1662 = ORIENTED_EDGE ( 'NONE', *, *, #1367, .F. ) ;
#1663 =( NAMED_UNIT ( * ) PLANE_ANGLE_UNIT ( ) SI_UNIT ( $, .RADIAN. ) );
#1664 = CARTESIAN_POINT ( 'NONE',  ( -12.50000000000000000, 1.530808498934191521E-15, 2.500000000000085265 ) ) ;
#1665 = PLANE ( 'NONE',  #4397 ) ;
#1666 = CARTESIAN_POINT ( 'NONE',  ( -37.49999999999994316, 225.0000000000000284, 0.000000000000000000 ) ) ;
#1667 = ORIENTED_EDGE ( 'NONE', *, *, #6328, .F. ) ;
#1668 = PRODUCT_DEFINITION_CONTEXT ( 'detailed design', #3218, 'design' ) ;
#1669 = ORIENTED_EDGE ( 'NONE', *, *, #4014, .F. ) ;
#1670 = ORIENTED_EDGE ( 'NONE', *, *, #6185, .F. ) ;
#1671 = ADVANCED_FACE ( 'NONE', ( #7000 ), #5839, .F. ) ;
#1672 = SURFACE_SIDE_STYLE ('',( #5317 ) ) ;
#1673 = DIRECTION ( 'NONE',  ( -1.000000000000000000, -0.000000000000000000, -0.000000000000000000 ) ) ;
#1674 = ORIENTED_EDGE ( 'NONE', *, *, #483, .T. ) ;
#1675 = SURFACE_SIDE_STYLE ('',( #7178 ) ) ;
#1676 = DIRECTION ( 'NONE',  ( -0.000000000000000000, -0.000000000000000000, -1.000000000000000000 ) ) ;
#1677 = VERTEX_POINT ( 'NONE', #7635 ) ;
#1678 = DIRECTION ( 'NONE',  ( 0.000000000000000000, 0.000000000000000000, 1.000000000000000000 ) ) ;
#1679 = EDGE_LOOP ( 'NONE', ( #277, #5855, #7443, #6655 ) ) ;
#1680 = DIRECTION ( 'NONE',  ( -1.000000000000000000, -0.000000000000000000, -0.000000000000000000 ) ) ;
#1681 = EDGE_LOOP ( 'NONE', ( #6131, #1576, #6775, #2352 ) ) ;
#1682 = DIRECTION ( 'NONE',  ( -0.000000000000000000, -0.000000000000000000, -1.000000000000000000 ) ) ;
#1683 = CARTESIAN_POINT ( 'NONE',  ( 150.0000000000000000, 1.836970198721029747E-14, 0.000000000000000000 ) ) ;
#1684 = PRODUCT_DEFINITION_FORMATION_WITH_SPECIFIED_SOURCE ( 'ANY', '', #6933, .NOT_KNOWN. ) ;
#1685 = ORIENTED_EDGE ( 'NONE', *, *, #6692, .F. ) ;
#1686 = ORIENTED_EDGE ( 'NONE', *, *, #6363, .T. ) ;
#1687 = PRODUCT_DEFINITION_SHAPE ( 'NONE', 'NONE',  #7925 ) ;
#1688 = CARTESIAN_POINT ( 'NONE',  ( 0.000000000000000000, -5.595828947448873159, 12.50000000000000000 ) ) ;
#1689 = DIRECTION ( 'NONE',  ( 0.000000000000000000, -0.000000000000000000, -1.000000000000000000 ) ) ;
#1690 = DIRECTION ( 'NONE',  ( 0.000000000000000000, 1.000000000000000000, 0.000000000000000000 ) ) ;
#1691 = CARTESIAN_POINT ( 'NONE',  ( 0.000000000000000000, 0.000000000000000000, 0.000000000000000000 ) ) ;
#1692 = CARTESIAN_POINT ( 'NONE',  ( 379.4971731025975146, 16.24331487217730796, -11.67016537472322746 ) ) ;
#1693 = EDGE_CURVE ( 'NONE', #1194, #4540, #6589, .T. ) ;
#1694 = EDGE_CURVE ( 'NONE', #2973, #6773, #7749, .T. ) ;
#1695 = CYLINDRICAL_SURFACE ( 'NONE', #5365, 25.00000000000000000 ) ;
#1696 =( LENGTH_UNIT ( ) NAMED_UNIT ( * ) SI_UNIT ( .MILLI., .METRE. ) );
#1697 = ORIENTED_EDGE ( 'NONE', *, *, #1694, .T. ) ;
#1698 =( NAMED_UNIT ( * ) SI_UNIT ( $, .STERADIAN. ) SOLID_ANGLE_UNIT ( ) );
#1699 = DIRECTION ( 'NONE',  ( 1.000000000000000000, 0.000000000000000000, 0.000000000000000000 ) ) ;
#1700 = FACE_OUTER_BOUND ( 'NONE', #184, .T. ) ;
#1701 = CARTESIAN_POINT ( 'NONE',  ( 12.50000000000000000, -24.99999999999999645, 3.851859888774471706E-31 ) ) ;
#1702 = ORIENTED_EDGE ( 'NONE', *, *, #5682, .F. ) ;
#1703 = ORIENTED_EDGE ( 'NONE', *, *, #1553, .T. ) ;
#1704 = VERTEX_POINT ( 'NONE', #1666 ) ;
#1705 = DIRECTION ( 'NONE',  ( 1.000000000000000000, -0.000000000000000000, 0.000000000000000000 ) ) ;
#1706 = ORIENTED_EDGE ( 'NONE', *, *, #2435, .F. ) ;
#1707 = CARTESIAN_POINT ( 'NONE',  ( 350.0000000000001137, -6.123233995736758985E-15, 25.00000000000000000 ) ) ;
#1708 = AXIS2_PLACEMENT_3D ( 'NONE', #1750, #7290, #7212 ) ;
#1709 = ADVANCED_FACE ( 'NONE', ( #2100, #2790, #7077, #2871, #3477, #7597 ), #5225, .T. ) ;
#1710 = ORIENTED_EDGE ( 'NONE', *, *, #809, .F. ) ;
#1711 = CIRCLE ( 'NONE', #6458, 65.50000000000000000 ) ;
#1712 = DIRECTION ( 'NONE',  ( -0.000000000000000000, -1.000000000000000000, -0.000000000000000000 ) ) ;
#1713 = EDGE_LOOP ( 'NONE', ( #7465, #7482 ) ) ;
#1714 = AXIS2_PLACEMENT_3D ( 'NONE', #779, #2551, #3232 ) ;
#1715 = CARTESIAN_POINT ( 'NONE',  ( 370.9025538143762901, -16.13667248250984798, 11.81655595281366899 ) ) ;
#1716 = ORIENTED_EDGE ( 'NONE', *, *, #6422, .F. ) ;
#1717 = CARTESIAN_POINT ( 'NONE',  ( 12.99038105676657651, -1.301042606982605321E-15, 0.000000000000000000 ) ) ;
#1718 = DIRECTION ( 'NONE',  ( -1.000000000000000000, -0.000000000000000000, -0.000000000000000000 ) ) ;
#1719 = VECTOR ( 'NONE', #6239, 1000.000000000000000 ) ;
#1720 = ORIENTED_EDGE ( 'NONE', *, *, #7865, .T. ) ;
#1721 = ORIENTED_EDGE ( 'NONE', *, *, #6028, .F. ) ;
#1722 = VECTOR ( 'NONE', #5401, 1000.000000000000000 ) ;
#1723 = VECTOR ( 'NONE', #6712, 1000.000000000000000 ) ;
#1724 = AXIS2_PLACEMENT_3D ( 'NONE', #209, #6989, #2658 ) ;
#1725 = CARTESIAN_POINT ( 'NONE',  ( -49.28095584970496645, 12.70544120911856112, 0.000000000000000000 ) ) ;
#1726 = LINE ( 'NONE', #6029, #7669 ) ;
#1727 = DIRECTION ( 'NONE',  ( 1.000000000000000000, -0.000000000000000000, -0.000000000000000000 ) ) ;
#1728 = EDGE_CURVE ( 'NONE', #155, #4944, #581, .T. ) ;
#1729 = DIRECTION ( 'NONE',  ( 1.000000000000000000, 0.000000000000000000, 0.000000000000000000 ) ) ;
#1730 = CARTESIAN_POINT ( 'NONE',  ( 383.5484565773660393, 17.79791451299709948, -9.128686039268288255 ) ) ;
#1731 = CIRCLE ( 'NONE', #2632, 5.000000000000000888 ) ;
#1732 = CARTESIAN_POINT ( 'NONE',  ( -0.000000000000000000, 87.70544117646394966, 0.000000000000000000 ) ) ;
#1733 = PRODUCT_CONTEXT ( 'NONE', #2591, 'mechanical' ) ;
#1734 = ADVANCED_FACE ( 'NONE', ( #3511 ), #4105, .T. ) ;
#1735 = SURFACE_STYLE_USAGE ( .BOTH. , #1816 ) ;
#1736 = DIRECTION ( 'NONE',  ( 0.000000000000000000, 1.000000000000000000, 0.000000000000000000 ) ) ;
#1738 = FACE_OUTER_BOUND ( 'NONE', #5355, .T. ) ;
#1737 = VECTOR ( 'NONE', #7454, 1000.000000000000000 ) ;
#1739 = DIRECTION ( 'NONE',  ( -0.000000000000000000, -0.000000000000000000, -1.000000000000000000 ) ) ;
#1740 = ORIENTED_EDGE ( 'NONE', *, *, #3722, .T. ) ;
#1741 = EDGE_CURVE ( 'NONE', #6534, #7849, #3015, .T. ) ;
#1742 = ORIENTED_EDGE ( 'NONE', *, *, #4873, .F. ) ;
#1743 = MANIFOLD_SOLID_BREP ( 'Pah1', #7475 ) ;
#1744 = ORIENTED_EDGE ( 'NONE', *, *, #3921, .T. ) ;
#1745 = ADVANCED_FACE ( 'NONE', ( #2347 ), #6560, .T. ) ;
#1746 = ORIENTED_EDGE ( 'NONE', *, *, #5161, .T. ) ;
#1747 = EDGE_CURVE ( 'NONE', #1519, #3303, #2106, .T. ) ;
#1748 = DIRECTION ( 'NONE',  ( 0.000000000000000000, 0.000000000000000000, -1.000000000000000000 ) ) ;
#1749 = FACE_OUTER_BOUND ( 'NONE', #3812, .T. ) ;
#1750 = CARTESIAN_POINT ( 'NONE',  ( -6.495190528383287365, 11.25000000000000000, 7.500000000000000000 ) ) ;
#1751 = ORIENTED_EDGE ( 'NONE', *, *, #5908, .F. ) ;
#1752 = AXIS2_PLACEMENT_3D ( 'NONE', #5760, #3385, #7162 ) ;
#1753 = CARTESIAN_POINT ( 'NONE',  ( 52.50000000000000711, 112.5000000000000142, 195.4980915752512658 ) ) ;
#1754 = ORIENTED_EDGE ( 'NONE', *, *, #1890, .T. ) ;
#1755 = FACE_OUTER_BOUND ( 'NONE', #922, .T. ) ;
#1756 = ORIENTED_EDGE ( 'NONE', *, *, #2718, .T. ) ;
#1757 = CARTESIAN_POINT ( 'NONE',  ( 362.8306064000756805, -19.79494591053120445, -2.886379146895018177 ) ) ;
#1758 = EDGE_LOOP ( 'NONE', ( #5121, #1183, #2583, #4790, #4354, #427, #2179, #5281 ) ) ;
#1759 = LINE ( 'NONE', #2405, #6658 ) ;
#1760 = CARTESIAN_POINT ( 'NONE',  ( 0.000000000000000000, 0.000000000000000000, 0.000000000000000000 ) ) ;
#1761 = ORIENTED_EDGE ( 'NONE', *, *, #1960, .F. ) ;
#1762 = ORIENTED_EDGE ( 'NONE', *, *, #1741, .F. ) ;
#1763 = CIRCLE ( 'NONE', #6514, 25.00000000000000000 ) ;
#1764 = CIRCLE ( 'NONE', #6769, 25.00000000000002132 ) ;
#1765 = DIRECTION ( 'NONE',  ( 0.000000000000000000, 0.000000000000000000, 1.000000000000000000 ) ) ;
#1766 = EDGE_CURVE ( 'NONE', #3409, #4567, #1781, .T. ) ;
#1767 = CARTESIAN_POINT ( 'NONE',  ( -31.24999999999997158, 47.50000000000009237, 195.5000000000000000 ) ) ;
#1768 = DIRECTION ( 'NONE',  ( 0.000000000000000000, 1.000000000000000000, -0.000000000000000000 ) ) ;
#1769 = LINE ( 'NONE', #6667, #6060 ) ;
#1770 = DIRECTION ( 'NONE',  ( -0.8660254037844387076, 0.5000000000000001110, 0.000000000000000000 ) ) ;
#1771 = CARTESIAN_POINT ( 'NONE',  ( 52.50000000000000711, 47.50000000000003553, 5.000000000000000000 ) ) ;
#1772 = SHAPE_REPRESENTATION ( 'Bolt1', ( #5785 ), #1803 ) ;
#1773 = AXIS2_PLACEMENT_3D ( 'NONE', #790, #3241, #5691 ) ;
#1774 = CIRCLE ( 'NONE', #114, 15.64999999999999680 ) ;
#1775 = DIRECTION ( 'NONE',  ( 0.000000000000000000, 0.000000000000000000, 1.000000000000000000 ) ) ;
#1776 = PRODUCT_CONTEXT ( 'NONE', #3012, 'mechanical' ) ;
#1777 = AXIS2_PLACEMENT_3D ( 'NONE', #2379, #4219, #5466 ) ;
#1778 = CARTESIAN_POINT ( 'NONE',  ( 12.50000000000000000, -24.99999999999999645, -3.235013004037443297E-15 ) ) ;
#1779 = AXIS2_PLACEMENT_3D ( 'NONE', #1248, #650, #726 ) ;
#1780 = CARTESIAN_POINT ( 'NONE',  ( 296.6025403784439050, 75.00000000000007105, 125.0000000000000000 ) ) ;
#1781 = LINE ( 'NONE', #4780, #1342 ) ;
#1782 = ORIENTED_EDGE ( 'NONE', *, *, #5595, .F. ) ;
#1783 = AXIS2_PLACEMENT_3D ( 'NONE', #3355, #939, #4592 ) ;
#1784 = PRODUCT_RELATED_PRODUCT_CATEGORY ( 'part', '', ( #2776 ) ) ;
#1785 = VERTEX_POINT ( 'NONE', #6636 ) ;
#1786 = AXIS2_PLACEMENT_3D ( 'NONE', #6056, #7304, #1800 ) ;
#1787 = VERTEX_POINT ( 'NONE', #3717 ) ;
#1788 = CARTESIAN_POINT ( 'NONE',  ( 42.50000000000000000, 42.50000000000003553, 0.000000000000000000 ) ) ;
#1789 = DIRECTION ( 'NONE',  ( -0.000000000000000000, 0.000000000000000000, -1.000000000000000000 ) ) ;
#1790 = CARTESIAN_POINT ( 'NONE',  ( 199.9999999999998863, 262.5000000000000568, 12.50000000000000000 ) ) ;
#1791 = ORIENTED_EDGE ( 'NONE', *, *, #997, .F. ) ;
#1792 = DIRECTION ( 'NONE',  ( 0.000000000000000000, 0.000000000000000000, 1.000000000000000000 ) ) ;
#1793 = EDGE_CURVE ( 'NONE', #3990, #5178, #2428, .T. ) ;
#1794 = ORIENTED_EDGE ( 'NONE', *, *, #3903, .T. ) ;
#1795 = EDGE_CURVE ( 'NONE', #1942, #7523, #6090, .T. ) ;
#1796 = DIRECTION ( 'NONE',  ( -1.000000000000000000, -0.000000000000000000, -0.000000000000000000 ) ) ;
#1797 = ORIENTED_EDGE ( 'NONE', *, *, #7679, .F. ) ;
#1798 = CARTESIAN_POINT ( 'NONE',  ( 367.3584912393716309, -17.37175308249308969, 9.924386979199645964 ) ) ;
#1799 = ORIENTED_EDGE ( 'NONE', *, *, #4197, .T. ) ;
#1800 = DIRECTION ( 'NONE',  ( 1.000000000000000000, 0.000000000000000000, 0.000000000000000000 ) ) ;
#1801 = DIRECTION ( 'NONE',  ( 1.000000000000000000, 0.000000000000000000, 0.000000000000000000 ) ) ;
#1802 = EDGE_CURVE ( 'NONE', #2333, #7620, #5392, .T. ) ;
#1803 =( GEOMETRIC_REPRESENTATION_CONTEXT ( 3 ) GLOBAL_UNCERTAINTY_ASSIGNED_CONTEXT ( ( #4469 ) ) GLOBAL_UNIT_ASSIGNED_CONTEXT ( ( #1858, #6799, #4304 ) ) REPRESENTATION_CONTEXT ( 'NONE', 'WORKASPACE' ) );
#1804 = ORIENTED_EDGE ( 'NONE', *, *, #6562, .F. ) ;
#1805 = ORIENTED_EDGE ( 'NONE', *, *, #6404, .T. ) ;
#1806 = DIRECTION ( 'NONE',  ( 1.000000000000000000, 0.000000000000000000, 0.000000000000000000 ) ) ;
#1807 = DIRECTION ( 'NONE',  ( 1.000000000000000000, 0.000000000000000000, 0.000000000000000000 ) ) ;
#1808 = DIRECTION ( 'NONE',  ( 0.000000000000000000, -0.000000000000000000, -1.000000000000000000 ) ) ;
#1809 = DIRECTION ( 'NONE',  ( 1.000000000000000000, 1.480297366166874072E-15, 0.000000000000000000 ) ) ;
#1810 = PRODUCT_DEFINITION_FORMATION_WITH_SPECIFIED_SOURCE ( 'ANY', '', #7704, .NOT_KNOWN. ) ;
#1811 = CARTESIAN_POINT ( 'NONE',  ( 326.6025403784437913, 82.50000000000004263, 125.0000000000000000 ) ) ;
#1812 = CARTESIAN_POINT ( 'NONE',  ( 376.6960688664906911, 15.69870025322426699, -12.39168528959425331 ) ) ;
#1813 = ADVANCED_FACE ( 'NONE', ( #7204 ), #6675, .T. ) ;
#1814 = DIRECTION ( 'NONE',  ( -0.7071067811865474617, 0.000000000000000000, -0.7071067811865474617 ) ) ;
#1815 = APPLICATION_PROTOCOL_DEFINITION ( 'draft international standard', 'automotive_design', 1998, #244 ) ;
#1816 = SURFACE_SIDE_STYLE ('',( #4777 ) ) ;
#1817 = DIRECTION ( 'NONE',  ( 1.000000000000000000, 0.000000000000000000, 0.000000000000000000 ) ) ;
#1818 = PLANE ( 'NONE',  #6211 ) ;
#1819 = DIRECTION ( 'NONE',  ( -1.000000000000000000, 0.000000000000000000, 0.000000000000000000 ) ) ;
#1820 = VERTEX_POINT ( 'NONE', #15 ) ;
#1821 = CARTESIAN_POINT ( 'NONE',  ( -36.78095584970496645, -62.29455879088143888, 12.50000000000000000 ) ) ;
#1822 = DIRECTION ( 'NONE',  ( -0.000000000000000000, -0.000000000000000000, -1.000000000000000000 ) ) ;
#1823 = DIRECTION ( 'NONE',  ( 0.000000000000000000, -0.000000000000000000, 1.000000000000000000 ) ) ;
#1824 = PLANE ( 'NONE',  #7489 ) ;
#1825 = ORIENTED_EDGE ( 'NONE', *, *, #5650, .F. ) ;
#1826 = CARTESIAN_POINT ( 'NONE',  ( 338.3083524847281183, 217.5000000000000284, 168.7439889854708213 ) ) ;
#1827 = CARTESIAN_POINT ( 'NONE',  ( 365.6323756216988272, 18.20590005533475875, -8.286065263872075093 ) ) ;
#1828 = ORIENTED_EDGE ( 'NONE', *, *, #809, .T. ) ;
#1829 = CARTESIAN_POINT ( 'NONE',  ( 371.6902873359033492, -15.95485291322333588, 12.06092292949322520 ) ) ;
#1830 = VERTEX_POINT ( 'NONE', #5512 ) ;
#1831 = EDGE_CURVE ( 'NONE', #116, #6898, #4011, .T. ) ;
#1832 = CARTESIAN_POINT ( 'NONE',  ( -24.28095581706361372, 2.657566677470048251E-15, 12.50000000000000000 ) ) ;
#1833 = FACE_OUTER_BOUND ( 'NONE', #3227, .T. ) ;
#1834 = EDGE_CURVE ( 'NONE', #1477, #2101, #6075, .T. ) ;
#1835 = ORIENTED_EDGE ( 'NONE', *, *, #6158, .T. ) ;
#1836 = ORIENTED_EDGE ( 'NONE', *, *, #7458, .F. ) ;
#1837 = EDGE_CURVE ( 'NONE', #6805, #4679, #7093, .T. ) ;
#1838 = ADVANCED_FACE ( 'NONE', ( #7321 ), #7241, .T. ) ;
#1839 = ORIENTED_EDGE ( 'NONE', *, *, #5026, .T. ) ;
#1840 = CARTESIAN_POINT ( 'NONE',  ( 13.21904415029503355, 62.70544120911855401, 12.50000000000000000 ) ) ;
#1841 = DIRECTION ( 'NONE',  ( -0.000000000000000000, -0.000000000000000000, -1.000000000000000000 ) ) ;
#1842 = DIRECTION ( 'NONE',  ( -1.000000000000000000, -0.000000000000000000, -0.000000000000000000 ) ) ;
#1843 = DIRECTION ( 'NONE',  ( -0.000000000000000000, -0.000000000000000000, -1.000000000000000000 ) ) ;
#1844 = AXIS2_PLACEMENT_3D ( 'NONE', #3707, #6301, #5541 ) ;
#1845 = AXIS2_PLACEMENT_3D ( 'NONE', #1905, #743, #4380 ) ;
#1846 = CARTESIAN_POINT ( 'NONE',  ( 398.0000000000001137, -12.50000000000000000, 15.61249499599599488 ) ) ;
#1847 = CIRCLE ( 'NONE', #3019, 11.49999999999995914 ) ;
#1848 = VECTOR ( 'NONE', #5787, 1000.000000000000000 ) ;
#1849 = AXIS2_PLACEMENT_3D ( 'NONE', #6710, #5017, #6116 ) ;
#1850 = CARTESIAN_POINT ( 'NONE',  ( 400.0000000000000000, -12.50000000000000000, 12.95183384698871620 ) ) ;
#1851 = CARTESIAN_POINT ( 'NONE',  ( 375.0000000000000000, -15.61249499599599488, 12.50000000000000711 ) ) ;
#1852 = DIRECTION ( 'NONE',  ( 0.4463453945640545317, 0.000000000000000000, -0.8948607650084221543 ) ) ;
#1853 = CARTESIAN_POINT ( 'NONE',  ( 25.00000000000000000, 0.000000000000000000, 0.000000000000000000 ) ) ;
#1854 = DIRECTION ( 'NONE',  ( 0.8660254037844383745, -0.5000000000000004441, 0.000000000000000000 ) ) ;
#1855 = CIRCLE ( 'NONE', #2503, 12.49999999999999822 ) ;
#1856 = ORIENTED_EDGE ( 'NONE', *, *, #4990, .F. ) ;
#1857 = VECTOR ( 'NONE', #5171, 1000.000000000000000 ) ;
#1858 =( LENGTH_UNIT ( ) NAMED_UNIT ( * ) SI_UNIT ( .MILLI., .METRE. ) );
#1859 = VERTEX_POINT ( 'NONE', #7359 ) ;
#1860 = SURFACE_SIDE_STYLE ('',( #7364 ) ) ;
#1861 = DIRECTION ( 'NONE',  ( -1.000000000000000000, 4.270088556250607616E-16, -0.000000000000000000 ) ) ;
#1862 = CARTESIAN_POINT ( 'NONE',  ( 25.00000000000000000, 0.000000000000000000, 0.000000000000000000 ) ) ;
#1863 = EDGE_CURVE ( 'NONE', #3875, #6273, #6600, .T. ) ;
#1864 = FACE_OUTER_BOUND ( 'NONE', #5811, .T. ) ;
#1865 = ORIENTED_EDGE ( 'NONE', *, *, #1600, .T. ) ;
#1866 = CARTESIAN_POINT ( 'NONE',  ( 12.50000000000000000, 1.530808498934191521E-15, 6.999999999999999112 ) ) ;
#1867 = VERTEX_POINT ( 'NONE', #1701 ) ;
#1868 = CARTESIAN_POINT ( 'NONE',  ( 374.5752787360723914, 15.61249499599598956, 12.50000000000000533 ) ) ;
#1869 = ORIENTED_EDGE ( 'NONE', *, *, #735, .T. ) ;
#1870 = CARTESIAN_POINT ( 'NONE',  ( 362.9351699716481221, -19.73070161726337446, -3.295910870315892804 ) ) ;
#1871 = AXIS2_PLACEMENT_3D ( 'NONE', #6161, #4993, #2549 ) ;
#1872 = VERTEX_POINT ( 'NONE', #4141 ) ;
#1873 = CARTESIAN_POINT ( 'NONE',  ( 2.775557561562891351E-14, 225.0000000000000284, 0.000000000000000000 ) ) ;
#1874 = CYLINDRICAL_SURFACE ( 'NONE', #2887, 32.75000000000001421 ) ;
#1875 = AXIS2_PLACEMENT_3D ( 'NONE', #4378, #5105, #6236 ) ;
#1876 = EDGE_LOOP ( 'NONE', ( #4967, #6168, #7080, #5452 ) ) ;
#1877 = PRODUCT_DEFINITION ( 'UNKNOWN', '', #913, #5431 ) ;
#1878 = ORIENTED_EDGE ( 'NONE', *, *, #980, .T. ) ;
#1879 = ORIENTED_EDGE ( 'NONE', *, *, #2482, .T. ) ;
#1880 = ADVANCED_FACE ( 'NONE', ( #1140 ), #6117, .F. ) ;
#1881 = PRODUCT_DEFINITION_SHAPE ( 'NONE', 'NONE',  #7933 ) ;
#1882 = PLANE ( 'NONE',  #352 ) ;
#1883 = DIRECTION ( 'NONE',  ( 0.000000000000000000, 0.000000000000000000, 1.000000000000000000 ) ) ;
#1884 = CARTESIAN_POINT ( 'NONE',  ( 0.000000000000000000, 4.382085397712380109E-15, -35.78244274809159720 ) ) ;
#1886 = LINE ( 'NONE', #727, #2593 ) ;
#1885 = VECTOR ( 'NONE', #253, 1000.000000000000000 ) ;
#1887 = CARTESIAN_POINT ( 'NONE',  ( 38.21904415029501934, 62.70544120911855401, 12.50000000000000000 ) ) ;
#1888 = EDGE_CURVE ( 'NONE', #4997, #3351, #1961, .T. ) ;
#1889 = VECTOR ( 'NONE', #6664, 1000.000000000000000 ) ;
#1890 = EDGE_CURVE ( 'NONE', #1554, #4302, #587, .T. ) ;
#1891 = SHAPE_DEFINITION_REPRESENTATION ( #5269, #3730 ) ;
#1892 = CARTESIAN_POINT ( 'NONE',  ( 0.7190441666157093570, -30.59582893112819946, 12.50000000000000000 ) ) ;
#1893 = LINE ( 'NONE', #2539, #1266 ) ;
#1894 = DIRECTION ( 'NONE',  ( -4.789677997474686366E-16, -1.000000000000000000, 0.000000000000000000 ) ) ;
#1895 = CYLINDRICAL_SURFACE ( 'NONE', #6216, 25.00000000000000000 ) ;
#1896 = AXIS2_PLACEMENT_3D ( 'NONE', #1904, #1822, #2624 ) ;
#1897 = EDGE_CURVE ( 'NONE', #5251, #4917, #621, .T. ) ;
#1898 = ADVANCED_FACE ( 'NONE', ( #1260, #4301 ), #1298, .F. ) ;
#1899 = EDGE_LOOP ( 'NONE', ( #2834, #4073, #1856, #4123 ) ) ;
#1900 = VECTOR ( 'NONE', #4296, 1000.000000000000114 ) ;
#1901 = AXIS2_PLACEMENT_3D ( 'NONE', #2696, #5826, #924 ) ;
#1902 = EDGE_LOOP ( 'NONE', ( #1828, #4886 ) ) ;
#1903 = FACE_OUTER_BOUND ( 'NONE', #5737, .T. ) ;
#1904 = CARTESIAN_POINT ( 'NONE',  ( 291.6025403784437913, 135.0000000000000000, 12.50000000000000000 ) ) ;
#1905 = CARTESIAN_POINT ( 'NONE',  ( 6.602357126051254174E-16, 0.000000000000000000, 0.000000000000000000 ) ) ;
#1906 = CARTESIAN_POINT ( 'NONE',  ( -49.28095584970496645, 12.70544120911856112, 12.50000000000000000 ) ) ;
#1907 = ORIENTED_EDGE ( 'NONE', *, *, #7596, .T. ) ;
#1908 = LINE ( 'NONE', #23, #838 ) ;
#1909 = AXIS2_PLACEMENT_3D ( 'NONE', #7258, #484, #4839 ) ;
#1910 = VECTOR ( 'NONE', #5503, 1000.000000000000000 ) ;
#1911 = EDGE_CURVE ( 'NONE', #957, #4302, #6950, .T. ) ;
#1912 = CARTESIAN_POINT ( 'NONE',  ( 368.6844851971966932, 16.83062759343247805, 10.81672997705310557 ) ) ;
#1913 = ORIENTED_EDGE ( 'NONE', *, *, #717, .T. ) ;
#1914 = DIRECTION ( 'NONE',  ( -1.000000000000000000, 1.224646799147353454E-16, 0.000000000000000000 ) ) ;
#1915 = ORIENTED_EDGE ( 'NONE', *, *, #5391, .F. ) ;
#1916 = PLANE ( 'NONE',  #5745 ) ;
#1917 = DIRECTION ( 'NONE',  ( -4.237492460401359023E-16, -1.000000000000000000, 0.000000000000000000 ) ) ;
#1918 = VERTEX_POINT ( 'NONE', #1333 ) ;
#1919 = VERTEX_POINT ( 'NONE', #3189 ) ;
#1920 = ORIENTED_EDGE ( 'NONE', *, *, #6916, .F. ) ;
#1921 = APPLICATION_CONTEXT ( 'automotive_design' ) ;
#1922 = DIRECTION ( 'NONE',  ( 1.000000000000000000, 0.000000000000000000, 0.000000000000000000 ) ) ;
#1923 = CARTESIAN_POINT ( 'NONE',  ( 384.8801577923950390, -18.47484582708395706, -7.667708004838452496 ) ) ;
#1924 = CARTESIAN_POINT ( 'NONE',  ( -12.50000000000000000, 0.000000000000000000, 0.000000000000000000 ) ) ;
#1925 = DIRECTION ( 'NONE',  ( 1.000000000000000000, 0.000000000000000000, 0.000000000000000000 ) ) ;
#1926 = DIRECTION ( 'NONE',  ( -0.000000000000000000, -0.000000000000000000, -1.000000000000000000 ) ) ;
#1927 = PRODUCT_CONTEXT ( 'NONE', #3162, 'mechanical' ) ;
#1928 = CIRCLE ( 'NONE', #6549, 5.000000000000004441 ) ;
#1929 = DIRECTION ( 'NONE',  ( 0.000000000000000000, 1.000000000000000000, 0.000000000000000000 ) ) ;
#1930 = LINE ( 'NONE', #3032, #5621 ) ;
#1931 = FACE_BOUND ( 'NONE', #6605, .T. ) ;
#1932 = EDGE_CURVE ( 'NONE', #5833, #4850, #6308, .T. ) ;
#1933 = ADVANCED_FACE ( 'NONE', ( #3151 ), #7474, .T. ) ;
#1934 = AXIS2_PLACEMENT_3D ( 'NONE', #1496, #3978, #7630 ) ;
#1935 = ORIENTED_EDGE ( 'NONE', *, *, #6757, .F. ) ;
#1936 = VERTEX_POINT ( 'NONE', #2616 ) ;
#1937 = CARTESIAN_POINT ( 'NONE',  ( 25.00000000000000000, -25.00000000000000000, 50.00000000000000000 ) ) ;
#1938 = FACE_OUTER_BOUND ( 'NONE', #5083, .T. ) ;
#1939 = DIRECTION ( 'NONE',  ( 1.000000000000000000, 0.000000000000000000, 0.000000000000000000 ) ) ;
#1940 = EDGE_CURVE ( 'NONE', #1161, #6259, #4667, .T. ) ;
#1941 = CARTESIAN_POINT ( 'NONE',  ( 0.000000000000000000, 0.000000000000000000, 77.49999999999998579 ) ) ;
#1942 = VERTEX_POINT ( 'NONE', #5097 ) ;
#1943 = DIRECTION ( 'NONE',  ( -0.000000000000000000, -1.000000000000000000, -0.000000000000000000 ) ) ;
#1944 = EDGE_LOOP ( 'NONE', ( #706, #7871, #5535, #5122 ) ) ;
#1945 = CARTESIAN_POINT ( 'NONE',  ( 374.1480243754402863, 15.61249499599599311, -12.50000000000000000 ) ) ;
#1946 = ORIENTED_EDGE ( 'NONE', *, *, #5665, .F. ) ;
#1947 = DIRECTION ( 'NONE',  ( -1.000000000000000000, 0.000000000000000000, 0.000000000000000000 ) ) ;
#1948 = ORIENTED_EDGE ( 'NONE', *, *, #4383, .F. ) ;
#1949 = CARTESIAN_POINT ( 'NONE',  ( 340.0000000000000000, 12.50000000000000000, -21.65063509461096913 ) ) ;
#1950 = LINE ( 'NONE', #6214, #1465 ) ;
#1951 = ADVANCED_FACE ( 'NONE', ( #734 ), #2579, .F. ) ;
#1952 = ORIENTED_EDGE ( 'NONE', *, *, #5255, .F. ) ;
#1953 = ORIENTED_EDGE ( 'NONE', *, *, #3393, .T. ) ;
#1954 = ORIENTED_EDGE ( 'NONE', *, *, #1793, .T. ) ;
#1955 = CARTESIAN_POINT ( 'NONE',  ( -25.00000000000000000, -25.00000000000000000, 50.00000000000000000 ) ) ;
#1956 = CARTESIAN_POINT ( 'NONE',  ( 0.000000000000000000, 25.00000000000000000, 25.00000000000000000 ) ) ;
#1957 = PLANE ( 'NONE',  #4195 ) ;
#1958 = EDGE_LOOP ( 'NONE', ( #1685, #4764, #5104, #1952 ) ) ;
#1959 = LINE ( 'NONE', #6867, #5164 ) ;
#1960 = EDGE_CURVE ( 'NONE', #5119, #107, #6232, .T. ) ;
#1961 = CIRCLE ( 'NONE', #1577, 24.99999999999999289 ) ;
#1962 = AXIS2_PLACEMENT_3D ( 'NONE', #1525, #7579, #6455 ) ;
#1963 = AXIS2_PLACEMENT_3D ( 'NONE', #7195, #5505, #5988 ) ;
#1964 = ITEM_DEFINED_TRANSFORMATION ( 'NONE', 'NONE', #2456,  #5785 ) ;
#1965 = AXIS2_PLACEMENT_3D ( 'NONE', #517, #3598, #6046 ) ;
#1966 = FACE_OUTER_BOUND ( 'NONE', #4644, .T. ) ;
#1967 = DIRECTION ( 'NONE',  ( 0.000000000000000000, 0.000000000000000000, 1.000000000000000000 ) ) ;
#1968 = CARTESIAN_POINT ( 'NONE',  ( 6.495190528383288253, -16.24999999999999645, 7.500000000000000000 ) ) ;
#1969 = CARTESIAN_POINT ( 'NONE',  ( 291.6025403784439050, 90.00000000000001421, 12.50000000000000000 ) ) ;
#1970 = AXIS2_PLACEMENT_3D ( 'NONE', #5204, #884, #3336 ) ;
#1971 = VECTOR ( 'NONE', #2615, 1000.000000000000000 ) ;
#1972 = EDGE_LOOP ( 'NONE', ( #5109, #4668, #3473, #2524 ) ) ;
#1973 = DIRECTION ( 'NONE',  ( 1.000000000000000000, 0.000000000000000000, 0.000000000000000000 ) ) ;
#1974 = ADVANCED_FACE ( 'NONE', ( #6194, #6830 ), #5594, .T. ) ;
#1975 =( REPRESENTATION_RELATIONSHIP ('NONE','NONE', #6292, #2073 ) REPRESENTATION_RELATIONSHIP_WITH_TRANSFORMATION ( #4860 )SHAPE_REPRESENTATION_RELATIONSHIP( ) );
#1976 = EDGE_LOOP ( 'NONE', ( #2884, #3176, #3092, #745 ) ) ;
#1977 = CARTESIAN_POINT ( 'NONE',  ( -9.381941874331415576, 16.25000000000000000, 7.500000000000000000 ) ) ;
#1978 = CARTESIAN_POINT ( 'NONE',  ( 0.000000000000000000, 0.000000000000000000, 97.50000000000000000 ) ) ;
#1979 = CARTESIAN_POINT ( 'NONE',  ( 0.000000000000000000, 177.5000000000000000, 12.50000000000000000 ) ) ;
#1980 = EDGE_CURVE ( 'NONE', #3124, #4547, #5637, .T. ) ;
#1981 = AXIS2_PLACEMENT_3D ( 'NONE', #5791, #3467, #289 ) ;
#1982 = DIRECTION ( 'NONE',  ( -4.270088556250607616E-16, -1.000000000000000000, 0.000000000000000000 ) ) ;
#1983 = ORIENTED_EDGE ( 'NONE', *, *, #1066, .F. ) ;
#1984 = DIRECTION ( 'NONE',  ( -0.000000000000000000, -0.000000000000000000, -1.000000000000000000 ) ) ;
#1985 = EDGE_CURVE ( 'NONE', #3684, #2973, #4498, .T. ) ;
#1986 = ADVANCED_FACE ( 'NONE', ( #4454 ), #91, .F. ) ;
#1987 = CARTESIAN_POINT ( 'NONE',  ( 362.9348919987150452, 19.73086988975742528, 3.295070860296623216 ) ) ;
#1988 = ORIENTED_EDGE ( 'NONE', *, *, #2635, .T. ) ;
#1989 = DIRECTION ( 'NONE',  ( 1.224646799147353207E-16, 1.000000000000000000, -0.000000000000000000 ) ) ;
#1990 = ORIENTED_EDGE ( 'NONE', *, *, #2007, .F. ) ;
#1991 = DIRECTION ( 'NONE',  ( 1.000000000000000000, 0.000000000000000000, 0.000000000000000000 ) ) ;
#1992 = CIRCLE ( 'NONE', #3153, 12.50000000000000000 ) ;
#1993 = LINE ( 'NONE', #3738, #4666 ) ;
#1994 = EDGE_CURVE ( 'NONE', #5786, #4514, #1221, .T. ) ;
#1995 = PRODUCT ( 'MAT-014', 'MAT-014', '', ( #1021 ) ) ;
#1996 = ORIENTED_EDGE ( 'NONE', *, *, #1747, .T. ) ;
#1997 = CIRCLE ( 'NONE', #7393, 25.00000000000000000 ) ;
#1998 = DIRECTION ( 'NONE',  ( -0.000000000000000000, 0.000000000000000000, 1.000000000000000000 ) ) ;
#1999 = VERTEX_POINT ( 'NONE', #6875 ) ;
#2000 = EDGE_LOOP ( 'NONE', ( #4198, #7225, #2547, #984 ) ) ;
#2001 = DIRECTION ( 'NONE',  ( 0.000000000000000000, -1.000000000000000000, 0.000000000000000000 ) ) ;
#2002 = CARTESIAN_POINT ( 'NONE',  ( 386.1839732711879378, -19.20325634068194631, -5.642343897998047808 ) ) ;
#2003 = CARTESIAN_POINT ( 'NONE',  ( 12.50000000000000355, 0.000000000000000000, 82.49999999999998579 ) ) ;
#2004 = VERTEX_POINT ( 'NONE', #7438 ) ;
#2005 = CARTESIAN_POINT ( 'NONE',  ( -12.50000000000000000, 0.000000000000000000, 45.00000000000000000 ) ) ;
#2006 = VECTOR ( 'NONE', #4742, 1000.000000000000000 ) ;
#2007 = EDGE_CURVE ( 'NONE', #2221, #2350, #3145, .T. ) ;
#2008 = VECTOR ( 'NONE', #2981, 1000.000000000000000 ) ;
#2009 = CONTEXT_DEPENDENT_SHAPE_REPRESENTATION ( #653, #3047 ) ;
#2010 = DIRECTION ( 'NONE',  ( 1.000000000000000000, 2.960594732333750117E-15, -0.000000000000000000 ) ) ;
#2011 = DIRECTION ( 'NONE',  ( 1.000000000000000000, 0.000000000000000000, 0.000000000000000000 ) ) ;
#2012 = CARTESIAN_POINT ( 'NONE',  ( 0.000000000000000000, 0.000000000000000000, 0.000000000000000000 ) ) ;
#2013 = DIRECTION ( 'NONE',  ( -0.000000000000000000, 1.000000000000000000, -0.000000000000000000 ) ) ;
#2014 = AXIS2_PLACEMENT_3D ( 'NONE', #2605, #2001, #4442 ) ;
#2015 = ORIENTED_EDGE ( 'NONE', *, *, #7776, .F. ) ;
#2016 = CARTESIAN_POINT ( 'NONE',  ( 0.000000000000000000, 0.000000000000000000, 45.00000000000000000 ) ) ;
#2017 = CARTESIAN_POINT ( 'NONE',  ( 303.6644303226275952, 147.1990734970208905, 230.9962291011628395 ) ) ;
#2018 = ORIENTED_EDGE ( 'NONE', *, *, #346, .F. ) ;
#2019 = AXIS2_PLACEMENT_3D ( 'NONE', #1405, #920, #6299 ) ;
#2020 = CARTESIAN_POINT ( 'NONE',  ( 50.71904415029504065, 62.70544120911855401, 0.000000000000000000 ) ) ;
#2021 = AXIS2_PLACEMENT_3D ( 'NONE', #5798, #816, #2140 ) ;
#2022 = DIRECTION ( 'NONE',  ( 1.000000000000000000, 0.000000000000000000, 0.000000000000000000 ) ) ;
#2023 = DIRECTION ( 'NONE',  ( 1.000000000000000000, 0.000000000000000000, 0.000000000000000000 ) ) ;
#2024 = VERTEX_POINT ( 'NONE', #5055 ) ;
#2025 = ADVANCED_FACE ( 'NONE', ( #4942 ), #1895, .F. ) ;
#2026 = CIRCLE ( 'NONE', #3069, 12.50000000000000000 ) ;
#2027 = AXIS2_PLACEMENT_3D ( 'NONE', #1778, #3509, #4222 ) ;
#2028 = FACE_OUTER_BOUND ( 'NONE', #3878, .T. ) ;
#2029 = ORIENTED_EDGE ( 'NONE', *, *, #6398, .F. ) ;
#2030 = DIRECTION ( 'NONE',  ( 0.000000000000000000, 0.000000000000000000, -1.000000000000000000 ) ) ;
#2031 = ORIENTED_EDGE ( 'NONE', *, *, #127, .T. ) ;
#2032 = CIRCLE ( 'NONE', #877, 12.50000000000000000 ) ;
#2033 = FACE_BOUND ( 'NONE', #3555, .T. ) ;
#2034 = AXIS2_PLACEMENT_3D ( 'NONE', #1924, #5461, #7389 ) ;
#2035 = DIRECTION ( 'NONE',  ( 0.000000000000000000, 0.000000000000000000, 1.000000000000000000 ) ) ;
#2036 = EDGE_CURVE ( 'NONE', #982, #6900, #771, .T. ) ;
#2037 = EDGE_CURVE ( 'NONE', #7527, #7631, #2757, .T. ) ;
#2038 = ORIENTED_EDGE ( 'NONE', *, *, #4734, .F. ) ;
#2039 = DIRECTION ( 'NONE',  ( -1.000000000000000000, 0.000000000000000000, 0.000000000000000000 ) ) ;
#2040 = ORIENTED_EDGE ( 'NONE', *, *, #4989, .F. ) ;
#2041 = VERTEX_POINT ( 'NONE', #7112 ) ;
#2042 = DIRECTION ( 'NONE',  ( -0.000000000000000000, -0.000000000000000000, -1.000000000000000000 ) ) ;
#2043 = FACE_OUTER_BOUND ( 'NONE', #4879, .T. ) ;
#2044 = ADVANCED_FACE ( 'NONE', ( #6386, #6990 ), #3301, .T. ) ;
#2045 = CARTESIAN_POINT ( 'NONE',  ( 398.6828372460798846, 12.50000000000000000, -14.73776325548316812 ) ) ;
#2046 = EDGE_CURVE ( 'NONE', #7248, #7215, #7873, .T. ) ;
#2047 = LINE ( 'NONE', #3971, #4662 ) ;
#2048 = CONTEXT_DEPENDENT_SHAPE_REPRESENTATION ( #5571, #5338 ) ;
#2049 = FACE_OUTER_BOUND ( 'NONE', #1594, .T. ) ;
#2050 = DIRECTION ( 'NONE',  ( 1.000000000000000000, 0.000000000000000000, 0.000000000000000000 ) ) ;
#2051 = CARTESIAN_POINT ( 'NONE',  ( 340.0000000000000000, 12.50000000000000000, 0.000000000000000000 ) ) ;
#2052 = CARTESIAN_POINT ( 'NONE',  ( 137.4999999999999716, 1.836970198721029747E-14, 25.00000000000000000 ) ) ;
#2053 = EDGE_CURVE ( 'NONE', #7250, #7782, #964, .T. ) ;
#2054 = ORIENTED_EDGE ( 'NONE', *, *, #7285, .T. ) ;
#2055 = LINE ( 'NONE', #6430, #7539 ) ;
#2056 = CARTESIAN_POINT ( 'NONE',  ( 124.0868394622074504, 189.1990734970206347, 183.2402661832477406 ) ) ;
#2057 = VERTEX_POINT ( 'NONE', #4012 ) ;
#2058 = FACE_OUTER_BOUND ( 'NONE', #1112, .T. ) ;
#2059 = FACE_OUTER_BOUND ( 'NONE', #4711, .T. ) ;
#2060 = CARTESIAN_POINT ( 'NONE',  ( -37.49999999999965183, -4.857225732735003066E-14, 12.50000000000000000 ) ) ;
#2061 = DIRECTION ( 'NONE',  ( -1.000000000000000000, 0.000000000000000000, 0.000000000000000000 ) ) ;
#2062 = ORIENTED_EDGE ( 'NONE', *, *, #1346, .F. ) ;
#2063 = PRODUCT_DEFINITION_SHAPE ( 'NONE', 'NONE',  #1877 ) ;
#2064 = AXIS2_PLACEMENT_3D ( 'NONE', #3427, #6556, #2953 ) ;
#2065 = VERTEX_POINT ( 'NONE', #3342 ) ;
#2066 = CARTESIAN_POINT ( 'NONE',  ( 190.0000000000000000, 0.000000000000000000, 0.000000000000000000 ) ) ;
#2067 = ORIENTED_EDGE ( 'NONE', *, *, #3718, .F. ) ;
#2068 = DIRECTION ( 'NONE',  ( -0.9335804380297002547, -0.3583679195021130526, -0.000000000000000000 ) ) ;
#2069 = DIRECTION ( 'NONE',  ( -1.000000000000000000, -0.000000000000000000, -0.000000000000000000 ) ) ;
#2070 = EDGE_CURVE ( 'NONE', #1787, #161, #5445, .T. ) ;
#2071 = FACE_OUTER_BOUND ( 'NONE', #4884, .T. ) ;
#2072 = PLANE ( 'NONE',  #3900 ) ;
#2073 = SHAPE_REPRESENTATION ( 'Connector', ( #5785 ), #5655 ) ;
#2074 = VECTOR ( 'NONE', #3182, 1000.000000000000000 ) ;
#2075 = ORIENTED_EDGE ( 'NONE', *, *, #3379, .F. ) ;
#2076 = LINE ( 'NONE', #7693, #4848 ) ;
#2077 = ORIENTED_EDGE ( 'NONE', *, *, #3083, .F. ) ;
#2078 = EDGE_CURVE ( 'NONE', #1102, #530, #6470, .T. ) ;
#2079 = ORIENTED_EDGE ( 'NONE', *, *, #6505, .T. ) ;
#2080 = DIRECTION ( 'NONE',  ( 0.000000000000000000, 0.000000000000000000, -1.000000000000000000 ) ) ;
#2081 = DIRECTION ( 'NONE',  ( 0.000000000000000000, 1.000000000000000000, 0.000000000000000000 ) ) ;
#2082 = ADVANCED_FACE ( 'NONE', ( #327 ), #2740, .F. ) ;
#2083 = DIRECTION ( 'NONE',  ( 1.000000000000000000, 0.000000000000000000, 0.000000000000000000 ) ) ;
#2084 = CIRCLE ( 'NONE', #6313, 20.00000000000000000 ) ;
#2085 = EDGE_CURVE ( 'NONE', #2565, #7589, #5866, .T. ) ;
#2086 = ORIENTED_EDGE ( 'NONE', *, *, #3997, .T. ) ;
#2087 = CARTESIAN_POINT ( 'NONE',  ( 0.000000000000000000, 0.000000000000000000, 97.50000000000000000 ) ) ;
#2088 = DIRECTION ( 'NONE',  ( -0.000000000000000000, -0.000000000000000000, 1.000000000000000000 ) ) ;
#2089 = CARTESIAN_POINT ( 'NONE',  ( 6.495190528383289141, -11.24999999999999645, 7.500000000000000000 ) ) ;
#2090 = CLOSED_SHELL ( 'NONE', ( #7775, #554, #5262, #7013, #7207, #2134, #3615, #3573, #3328, #375, #6010, #5268, #2334, #569, #598, #6964, #225, #5768, #2634, #2082, #5641 ) ) ;
#2091 = CARTESIAN_POINT ( 'NONE',  ( 296.6025403784439618, 217.5000000000000568, 125.0000000000000000 ) ) ;
#2092 = ORIENTED_EDGE ( 'NONE', *, *, #1985, .T. ) ;
#2093 = ADVANCED_FACE ( 'NONE', ( #3976 ), #370, .F. ) ;
#2094 = AXIS2_PLACEMENT_3D ( 'NONE', #1419, #3870, #858 ) ;
#2095 = CARTESIAN_POINT ( 'NONE',  ( 296.6025403784437913, 137.4999999999999716, 17.49999999999998934 ) ) ;
#2096 = ORIENTED_EDGE ( 'NONE', *, *, #6207, .T. ) ;
#2097 = PLANE ( 'NONE',  #7513 ) ;
#2098 = CARTESIAN_POINT ( 'NONE',  ( 339.1025403784437913, 82.50000000000004263, 125.0000000000000000 ) ) ;
#2099 = CARTESIAN_POINT ( 'NONE',  ( 296.6025403784437913, 87.50000000000005684, 17.49999999999998934 ) ) ;
#2100 = FACE_OUTER_BOUND ( 'NONE', #7135, .T. ) ;
#2101 = VERTEX_POINT ( 'NONE', #7666 ) ;
#2102 = VECTOR ( 'NONE', #4565, 1000.000000000000000 ) ;
#2103 = ORIENTED_EDGE ( 'NONE', *, *, #5241, .F. ) ;
#2104 = AXIS2_PLACEMENT_3D ( 'NONE', #7494, #6733, #4962 ) ;
#2105 = DIRECTION ( 'NONE',  ( 0.000000000000000000, 1.000000000000000000, 0.000000000000000000 ) ) ;
#2106 = CIRCLE ( 'NONE', #3658, 12.50000000000000000 ) ;
#2107 = ORIENTED_EDGE ( 'NONE', *, *, #1651, .T. ) ;
#2108 = CIRCLE ( 'NONE', #319, 65.50000000000000000 ) ;
#2109 = EDGE_CURVE ( 'NONE', #2387, #3363, #5907, .T. ) ;
#2110 = DIRECTION ( 'NONE',  ( 0.000000000000000000, -1.000000000000000000, 0.000000000000000000 ) ) ;
#2111 = CYLINDRICAL_SURFACE ( 'NONE', #6451, 15.00000000000000000 ) ;
#2112 = DIRECTION ( 'NONE',  ( 0.000000000000000000, 1.000000000000000000, 0.000000000000000000 ) ) ;
#2113 = LINE ( 'NONE', #4038, #6469 ) ;
#2114 = ORIENTED_EDGE ( 'NONE', *, *, #5066, .F. ) ;
#2115 = FACE_OUTER_BOUND ( 'NONE', #4804, .T. ) ;
#2116 = ORIENTED_EDGE ( 'NONE', *, *, #1612, .T. ) ;
#2117 = AXIS2_PLACEMENT_3D ( 'NONE', #5966, #3357, #4628 ) ;
#2118 = ORIENTED_EDGE ( 'NONE', *, *, #2314, .F. ) ;
#2119 = CARTESIAN_POINT ( 'NONE',  ( -37.49999999999965183, -4.857225732735003066E-14, 12.50000000000000000 ) ) ;
#2120 = DIRECTION ( 'NONE',  ( -0.000000000000000000, -0.000000000000000000, -1.000000000000000000 ) ) ;
#2121 = DIRECTION ( 'NONE',  ( -1.094506615593124476E-16, -1.000000000000000000, 0.000000000000000000 ) ) ;
#2122 = CYLINDRICAL_SURFACE ( 'NONE', #6718, 12.50000000000000355 ) ;
#2123 = PRODUCT_DEFINITION ( 'UNKNOWN', '', #1810, #4068 ) ;
#2124 = VECTOR ( 'NONE', #3680, 1000.000000000000000 ) ;
#2125 = EDGE_CURVE ( 'NONE', #2853, #2024, #6842, .T. ) ;
#2126 = VERTEX_POINT ( 'NONE', #1015 ) ;
#2127 = PRODUCT ( 'Rod', 'Rod', '', ( #1776 ) ) ;
#2128 = DIRECTION ( 'NONE',  ( 0.000000000000000000, 0.000000000000000000, -1.000000000000000000 ) ) ;
#2129 = CARTESIAN_POINT ( 'NONE',  ( 353.4483633286965301, 82.50000000000004263, 138.3903618369216417 ) ) ;
#2131 = LINE ( 'NONE', #770, #1083 ) ;
#2130 = AXIS2_PLACEMENT_3D ( 'NONE', #5914, #6474, #6997 ) ;
#2132 = DIRECTION ( 'NONE',  ( 1.000000000000000000, 0.000000000000000000, 0.000000000000000000 ) ) ;
#2133 = DIRECTION ( 'NONE',  ( 1.000000000000000000, 0.000000000000000000, 0.000000000000000000 ) ) ;
#2134 = ADVANCED_FACE ( 'NONE', ( #6512 ), #7754, .F. ) ;
#2135 = VECTOR ( 'NONE', #533, 1000.000000000000000 ) ;
#2136 = ADVANCED_FACE ( 'NONE', ( #2262 ), #2781, .F. ) ;
#2137 = DIRECTION ( 'NONE',  ( 1.000000000000000000, 0.000000000000000000, 0.000000000000000000 ) ) ;
#2138 = EDGE_LOOP ( 'NONE', ( #3240, #7117, #424, #2597 ) ) ;
#2139 = CARTESIAN_POINT ( 'NONE',  ( -8.959197987552832032, 23.33951095074251114, 25.00000000000000000 ) ) ;
#2140 = DIRECTION ( 'NONE',  ( 0.000000000000000000, 0.000000000000000000, -1.000000000000000000 ) ) ;
#2141 = LINE ( 'NONE', #3431, #6459 ) ;
#2142 = PRESENTATION_STYLE_ASSIGNMENT (( #5266 ) ) ;
#2143 = VERTEX_POINT ( 'NONE', #7031 ) ;
#2144 = EDGE_CURVE ( 'NONE', #322, #3264, #1535, .T. ) ;
#2145 = VECTOR ( 'NONE', #6417, 1000.000000000000000 ) ;
#2146 = VERTEX_POINT ( 'NONE', #5828 ) ;
#2147 = AXIS2_PLACEMENT_3D ( 'NONE', #2562, #3919, #3325 ) ;
#2148 = VECTOR ( 'NONE', #3681, 1000.000000000000000 ) ;
#2149 = CARTESIAN_POINT ( 'NONE',  ( 25.71904415029483459, 19.40417101989674009, 12.50000000000000000 ) ) ;
#2150 = VERTEX_POINT ( 'NONE', #2175 ) ;
#2151 = CARTESIAN_POINT ( 'NONE',  ( 75.00000000000000000, 10.56842436860067735, 25.00000000000000000 ) ) ;
#2152 = CARTESIAN_POINT ( 'NONE',  ( 41.25000000000002842, 47.34122918275932079, 12.50000000000000000 ) ) ;
#2153 = PRESENTATION_STYLE_ASSIGNMENT (( #4712 ) ) ;
#2154 = DIRECTION ( 'NONE',  ( 1.000000000000000000, 0.000000000000000000, 0.000000000000000000 ) ) ;
#2155 =( GEOMETRIC_REPRESENTATION_CONTEXT ( 3 ) GLOBAL_UNCERTAINTY_ASSIGNED_CONTEXT ( ( #6961 ) ) GLOBAL_UNIT_ASSIGNED_CONTEXT ( ( #4632, #909, #3359 ) ) REPRESENTATION_CONTEXT ( 'NONE', 'WORKASPACE' ) );
#2156 = VECTOR ( 'NONE', #3820, 1000.000000000000000 ) ;
#2157 = EDGE_CURVE ( 'NONE', #3721, #642, #4612, .T. ) ;
#2158 = EDGE_LOOP ( 'NONE', ( #3332, #7881 ) ) ;
#2159 = DIRECTION ( 'NONE',  ( 0.000000000000000000, 0.000000000000000000, 1.000000000000000000 ) ) ;
#2160 = EDGE_LOOP ( 'NONE', ( #1702, #5057 ) ) ;
#2161 = VECTOR ( 'NONE', #7054, 1000.000000000000000 ) ;
#2162 = CARTESIAN_POINT ( 'NONE',  ( 0.000000000000000000, 0.000000000000000000, 12.50000000000000000 ) ) ;
#2163 = CIRCLE ( 'NONE', #6649, 25.00000000000000000 ) ;
#2164 = ORIENTED_EDGE ( 'NONE', *, *, #1448, .F. ) ;
#2165 = DIRECTION ( 'NONE',  ( -0.000000000000000000, -0.000000000000000000, -1.000000000000000000 ) ) ;
#2166 = CARTESIAN_POINT ( 'NONE',  ( 50.71904415029504065, 87.70544117646394966, 0.000000000000000000 ) ) ;
#2167 = CARTESIAN_POINT ( 'NONE',  ( -10.82531754730547924, 13.75000000000000000, 0.000000000000000000 ) ) ;
#2168 = DIRECTION ( 'NONE',  ( 1.000000000000000000, 0.000000000000000000, 0.000000000000000000 ) ) ;
#2169 = CONICAL_SURFACE ( 'NONE', #5236, 11.64999999999996660, 0.7853981633974482790 ) ;
#2170 = VECTOR ( 'NONE', #1768, 1000.000000000000000 ) ;
#2171 = ORIENTED_EDGE ( 'NONE', *, *, #5582, .F. ) ;
#2172 = DIRECTION ( 'NONE',  ( 0.000000000000000000, -1.000000000000000000, -0.000000000000000000 ) ) ;
#2173 = FACE_BOUND ( 'NONE', #3436, .T. ) ;
#2174 = DIRECTION ( 'NONE',  ( 1.000000000000000000, 0.000000000000000000, 0.000000000000000000 ) ) ;
#2175 = CARTESIAN_POINT ( 'NONE',  ( 13.00000000000000178, 0.000000000000000000, 7.500000000000000000 ) ) ;
#2176 = CARTESIAN_POINT ( 'NONE',  ( 384.1017607431604688, 18.07018020958731697, 8.577132482464245200 ) ) ;
#2177 = CARTESIAN_POINT ( 'NONE',  ( -11.49999999999995914, 1.469576158976821383E-15, 0.000000000000000000 ) ) ;
#2178 = DIRECTION ( 'NONE',  ( 0.9847062208914363346, -4.715591380374466672E-16, -0.1742230138004330908 ) ) ;
#2179 = ORIENTED_EDGE ( 'NONE', *, *, #3656, .F. ) ;
#2180 = EDGE_CURVE ( 'NONE', #4623, #103, #7862, .T. ) ;
#2181 = CARTESIAN_POINT ( 'NONE',  ( 2.775557561562891351E-14, 225.0000000000000284, 12.50000000000000000 ) ) ;
#2182 = DIRECTION ( 'NONE',  ( -0.000000000000000000, 0.000000000000000000, 1.000000000000000000 ) ) ;
#2183 = CARTESIAN_POINT ( 'NONE',  ( 46.25000000000002842, 177.5000000000000000, 130.0000000000000000 ) ) ;
#2184 = APPLICATION_CONTEXT ( 'automotive_design' ) ;
#2185 = DIRECTION ( 'NONE',  ( -1.000000000000000000, -0.000000000000000000, -0.000000000000000000 ) ) ;
#2186 = VERTEX_POINT ( 'NONE', #6107 ) ;
#2187 = EDGE_CURVE ( 'NONE', #4661, #2323, #1129, .T. ) ;
#2188 = ORIENTED_EDGE ( 'NONE', *, *, #4350, .T. ) ;
#2189 = EDGE_CURVE ( 'NONE', #3802, #5551, #4769, .T. ) ;
#2190 = DIRECTION ( 'NONE',  ( -0.000000000000000000, -0.000000000000000000, -1.000000000000000000 ) ) ;
#2191 = ORIENTED_EDGE ( 'NONE', *, *, #3784, .F. ) ;
#2192 = PLANE ( 'NONE',  #2117 ) ;
#2193 = ORIENTED_EDGE ( 'NONE', *, *, #4457, .T. ) ;
#2194 = AXIS2_PLACEMENT_3D ( 'NONE', #2066, #5727, #4029 ) ;
#2195 = VERTEX_POINT ( 'NONE', #5946 ) ;
#2196 = CARTESIAN_POINT ( 'NONE',  ( 42.50000000000000711, 182.5000000000000000, 12.50000000000000000 ) ) ;
#2197 = DIRECTION ( 'NONE',  ( 1.000000000000000000, -3.469446951953614189E-17, 0.000000000000000000 ) ) ;
#2198 = PRODUCT ( 'V-Link', 'V-Link', '', ( #1328 ) ) ;
#2199 = LINE ( 'NONE', #6097, #1261 ) ;
#2200 = EDGE_LOOP ( 'NONE', ( #5796, #2704, #1121, #5767 ) ) ;
#2201 = LINE ( 'NONE', #7016, #7294 ) ;
#2202 = ORIENTED_EDGE ( 'NONE', *, *, #3027, .F. ) ;
#2203 = DIRECTION ( 'NONE',  ( 0.000000000000000000, 0.000000000000000000, -1.000000000000000000 ) ) ;
#2204 = EDGE_LOOP ( 'NONE', ( #7614, #2465 ) ) ;
#2205 = DIRECTION ( 'NONE',  ( 1.000000000000000000, 0.000000000000000000, 0.000000000000000000 ) ) ;
#2206 = EDGE_CURVE ( 'NONE', #5860, #600, #6586, .T. ) ;
#2207 = PRESENTATION_STYLE_ASSIGNMENT (( #961 ) ) ;
#2208 = LINE ( 'NONE', #4005, #1640 ) ;
#2209 = CARTESIAN_POINT ( 'NONE',  ( 353.4483633286965301, 142.5000000000000000, 138.3903618369216417 ) ) ;
#2210 = AXIS2_PLACEMENT_3D ( 'NONE', #2983, #458, #2904 ) ;
#2211 = EDGE_LOOP ( 'NONE', ( #863, #4082, #6575, #3883 ) ) ;
#2212 = VECTOR ( 'NONE', #3066, 1000.000000000000000 ) ;
#2213 = EDGE_CURVE ( 'NONE', #600, #3816, #2417, .T. ) ;
#2214 = CYLINDRICAL_SURFACE ( 'NONE', #7786, 12.50000000000001066 ) ;
#2215 = DIRECTION ( 'NONE',  ( -0.000000000000000000, -0.000000000000000000, -1.000000000000000000 ) ) ;
#2216 = CARTESIAN_POINT ( 'NONE',  ( 25.00000000000000000, 0.000000000000000000, -12.50000000000000000 ) ) ;
#2217 = CARTESIAN_POINT ( 'NONE',  ( 25.71904415029483459, 19.40417101989674009, 12.50000000000000000 ) ) ;
#2218 = FACE_OUTER_BOUND ( 'NONE', #1414, .T. ) ;
#2219 = CARTESIAN_POINT ( 'NONE',  ( 398.6828372460798846, 12.50000000000000000, 14.73776325548316812 ) ) ;
#2220 = DIRECTION ( 'NONE',  ( 4.789593822244094799E-16, 1.000000000000000000, 5.328524654824031087E-22 ) ) ;
#2221 = VERTEX_POINT ( 'NONE', #1091 ) ;
#2222 =( LENGTH_UNIT ( ) NAMED_UNIT ( * ) SI_UNIT ( .MILLI., .METRE. ) );
#2223 = CARTESIAN_POINT ( 'NONE',  ( 125.0000000000000000, 3.061616997868383043E-15, -25.00000000000000000 ) ) ;
#2224 = CARTESIAN_POINT ( 'NONE',  ( -26.24999999999997158, 47.34122918275937053, 12.50000000000000000 ) ) ;
#2225 =( NAMED_UNIT ( * ) PLANE_ANGLE_UNIT ( ) SI_UNIT ( $, .RADIAN. ) );
#2226 = VERTEX_POINT ( 'NONE', #7231 ) ;
#2227 = CIRCLE ( 'NONE', #179, 17.50000000000000355 ) ;
#2228 = UNCERTAINTY_MEASURE_WITH_UNIT (LENGTH_MEASURE( 1.000000000000000082E-05 ), #1696, 'distance_accuracy_value', 'NONE');
#2229 = VECTOR ( 'NONE', #5086, 1000.000000000000000 ) ;
#2230 = AXIS2_PLACEMENT_3D ( 'NONE', #4191, #7254, #4670 ) ;
#2231 = PRODUCT_DEFINITION ( 'UNKNOWN', '', #539, #7599 ) ;
#2232 = ORIENTED_EDGE ( 'NONE', *, *, #4981, .T. ) ;
#2233 = ADVANCED_FACE ( 'NONE', ( #4735 ), #3541, .F. ) ;
#2234 =( NAMED_UNIT ( * ) SI_UNIT ( $, .STERADIAN. ) SOLID_ANGLE_UNIT ( ) );
#2235 = ORIENTED_EDGE ( 'NONE', *, *, #2189, .F. ) ;
#2236 = CYLINDRICAL_SURFACE ( 'NONE', #3037, 12.49999999999999822 ) ;
#2238 = CARTESIAN_POINT ( 'NONE',  ( 12.50000000000000000, 0.000000000000000000, 0.000000000000000000 ) ) ;
#2237 = VECTOR ( 'NONE', #4368, 1000.000000000000000 ) ;
#2239 = CIRCLE ( 'NONE', #2094, 17.50000000000000355 ) ;
#2240 = ORIENTED_EDGE ( 'NONE', *, *, #4119, .F. ) ;
#2241 = DIRECTION ( 'NONE',  ( -0.000000000000000000, -0.000000000000000000, -1.000000000000000000 ) ) ;
#2242 = EDGE_CURVE ( 'NONE', #5920, #4944, #3890, .T. ) ;
#2243 = ADVANCED_FACE ( 'NONE', ( #537 ), #2457, .F. ) ;
#2244 = AXIS2_PLACEMENT_3D ( 'NONE', #5555, #1187, #58 ) ;
#2245 = ORIENTED_EDGE ( 'NONE', *, *, #134, .F. ) ;
#2246 = AXIS2_PLACEMENT_3D ( 'NONE', #6829, #90, #4300 ) ;
#2247 = DIRECTION ( 'NONE',  ( -0.000000000000000000, -0.000000000000000000, -1.000000000000000000 ) ) ;
#2248 = ORIENTED_EDGE ( 'NONE', *, *, #545, .F. ) ;
#2249 = CARTESIAN_POINT ( 'NONE',  ( 190.0000000000000000, 0.000000000000000000, 0.000000000000000000 ) ) ;
#2250 = ORIENTED_EDGE ( 'NONE', *, *, #2297, .F. ) ;
#2251 = CARTESIAN_POINT ( 'NONE',  ( 353.4483633286965301, 217.5000000000000284, 138.3903618369216417 ) ) ;
#2252 = DIRECTION ( 'NONE',  ( -0.000000000000000000, -0.000000000000000000, -1.000000000000000000 ) ) ;
#2253 = VECTOR ( 'NONE', #563, 1000.000000000000000 ) ;
#2254 = DIRECTION ( 'NONE',  ( 1.000000000000000000, 0.000000000000000000, 0.000000000000000000 ) ) ;
#2255 = EDGE_CURVE ( 'NONE', #4458, #5006, #1451, .T. ) ;
#2256 = ORIENTED_EDGE ( 'NONE', *, *, #3175, .T. ) ;
#2257 = AXIS2_PLACEMENT_3D ( 'NONE', #6008, #2241, #6050 ) ;
#2258 = ORIENTED_EDGE ( 'NONE', *, *, #5071, .F. ) ;
#2259 = FACE_OUTER_BOUND ( 'NONE', #5973, .T. ) ;
#2260 = CARTESIAN_POINT ( 'NONE',  ( -24.28095581706362083, -62.29455879088143888, 12.50000000000000000 ) ) ;
#2261 = CYLINDRICAL_SURFACE ( 'NONE', #6821, 65.50000000000000000 ) ;
#2262 = FACE_OUTER_BOUND ( 'NONE', #5325, .T. ) ;
#2263 = AXIS2_PLACEMENT_3D ( 'NONE', #2162, #7696, #7184 ) ;
#2264 = CARTESIAN_POINT ( 'NONE',  ( 376.6784352945268779, 15.68173745365923288, 12.41480524315420197 ) ) ;
#2265 = EDGE_CURVE ( 'NONE', #1785, #2355, #2227, .T. ) ;
#2266 = DIRECTION ( 'NONE',  ( 0.000000000000000000, 0.000000000000000000, -1.000000000000000000 ) ) ;
#2267 = PRESENTATION_LAYER_ASSIGNMENT (  '', '', ( #7383 ) ) ;
#2268 = PRODUCT_CONTEXT ( 'NONE', #1516, 'mechanical' ) ;
#2269 = VERTEX_POINT ( 'NONE', #4172 ) ;
#2270 = CARTESIAN_POINT ( 'NONE',  ( 32.53766565774834163, -18.78563002630307111, 12.50000000000000000 ) ) ;
#2271 = LINE ( 'NONE', #4699, #7540 ) ;
#2272 = CARTESIAN_POINT ( 'NONE',  ( -37.49999999999995026, 37.50000000000010658, 0.000000000000000000 ) ) ;
#2273 = DIRECTION ( 'NONE',  ( 1.000000000000000000, 0.000000000000000000, 0.000000000000000000 ) ) ;
#2274 = ORIENTED_EDGE ( 'NONE', *, *, #7240, .T. ) ;
#2275 = CIRCLE ( 'NONE', #3295, 12.50000000000000355 ) ;
#2276 = ORIENTED_EDGE ( 'NONE', *, *, #6309, .T. ) ;
#2277 = ORIENTED_EDGE ( 'NONE', *, *, #2573, .F. ) ;
#2278 =( NAMED_UNIT ( * ) PLANE_ANGLE_UNIT ( ) SI_UNIT ( $, .RADIAN. ) );
#2279 = ORIENTED_EDGE ( 'NONE', *, *, #1409, .F. ) ;
#2280 = PLANE ( 'NONE',  #2383 ) ;
#2281 = AXIS2_PLACEMENT_3D ( 'NONE', #7706, #5167, #2128 ) ;
#2282 = DIRECTION ( 'NONE',  ( 1.000000000000000000, 0.000000000000000000, 0.000000000000000000 ) ) ;
#2283 = ORIENTED_EDGE ( 'NONE', *, *, #2600, .F. ) ;
#2284 = CYLINDRICAL_SURFACE ( 'NONE', #3708, 5.000000000000004441 ) ;
#2285 = LINE ( 'NONE', #5971, #7373 ) ;
#2286 = AXIS2_PLACEMENT_3D ( 'NONE', #7698, #6499, #6644 ) ;
#2287 = ORIENTED_EDGE ( 'NONE', *, *, #1994, .F. ) ;
#2288 = CARTESIAN_POINT ( 'NONE',  ( 398.0000000000001137, 0.000000000000000000, 0.000000000000000000 ) ) ;
#2289 = ORIENTED_EDGE ( 'NONE', *, *, #7584, .T. ) ;
#2290 = CARTESIAN_POINT ( 'NONE',  ( 374.1528078369840387, -15.61249499599599844, 12.50000000000001066 ) ) ;
#2291 = ORIENTED_EDGE ( 'NONE', *, *, #7091, .T. ) ;
#2292 = VECTOR ( 'NONE', #4684, 1000.000000000000000 ) ;
#2293 = EDGE_CURVE ( 'NONE', #1872, #5638, #5944, .T. ) ;
#2294 = DIRECTION ( 'NONE',  ( -1.000000000000000000, 0.000000000000000000, 0.000000000000000000 ) ) ;
#2295 = VECTOR ( 'NONE', #2788, 1000.000000000000000 ) ;
#2296 = CYLINDRICAL_SURFACE ( 'NONE', #6979, 31.24999999999999289 ) ;
#2297 = EDGE_CURVE ( 'NONE', #3524, #4687, #4216, .T. ) ;
#2298 = EDGE_LOOP ( 'NONE', ( #3498, #5134, #4168, #7916 ) ) ;
#2299 = AXIS2_PLACEMENT_3D ( 'NONE', #2095, #3265, #7628 ) ;
#2300 = VECTOR ( 'NONE', #3626, 1000.000000000000000 ) ;
#2301 = EDGE_LOOP ( 'NONE', ( #7044, #3698 ) ) ;
#2302 = DIRECTION ( 'NONE',  ( 0.000000000000000000, 0.000000000000000000, -1.000000000000000000 ) ) ;
#2303 = CARTESIAN_POINT ( 'NONE',  ( 0.000000000000000000, 25.00000000000000000, 0.000000000000000000 ) ) ;
#2304 = CARTESIAN_POINT ( 'NONE',  ( 296.6025403784437913, 149.9999999999999716, 12.50000000000000000 ) ) ;
#2305 = PLANE ( 'NONE',  #5557 ) ;
#2306 = CIRCLE ( 'NONE', #3324, 12.50000000000001066 ) ;
#2307 = CARTESIAN_POINT ( 'NONE',  ( 387.4992068747945950, 19.99950429724430023, 0.4454306286988182761 ) ) ;
#2308 = PLANE ( 'NONE',  #502 ) ;
#2309 = CARTESIAN_POINT ( 'NONE',  ( 244.2840207499967278, 202.1990734970208337, 178.2402661832445006 ) ) ;
#2310 = ORIENTED_EDGE ( 'NONE', *, *, #4826, .F. ) ;
#2311 = CARTESIAN_POINT ( 'NONE',  ( -17.32050807568877104, -2.499999999999999556, 7.500000000000000000 ) ) ;
#2312 = DIRECTION ( 'NONE',  ( 0.000000000000000000, 0.000000000000000000, -1.000000000000000000 ) ) ;
#2313 = DIRECTION ( 'NONE',  ( 0.000000000000000000, 0.000000000000000000, 1.000000000000000000 ) ) ;
#2314 = EDGE_CURVE ( 'NONE', #3534, #7382, #2905, .T. ) ;
#2315 = DIRECTION ( 'NONE',  ( 1.000000000000000000, 0.000000000000000000, 0.000000000000000000 ) ) ;
#2316 = EDGE_LOOP ( 'NONE', ( #4599, #6248, #201, #5661 ) ) ;
#2317 = ORIENTED_EDGE ( 'NONE', *, *, #6348, .T. ) ;
#2318 =( NAMED_UNIT ( * ) SI_UNIT ( $, .STERADIAN. ) SOLID_ANGLE_UNIT ( ) );
#2319 = ORIENTED_EDGE ( 'NONE', *, *, #2984, .F. ) ;
#2320 = PLANE ( 'NONE',  #5560 ) ;
#2321 = VERTEX_POINT ( 'NONE', #1846 ) ;
#2322 = CARTESIAN_POINT ( 'NONE',  ( 0.000000000000000000, 0.000000000000000000, 47.50000000000000000 ) ) ;
#2323 = VERTEX_POINT ( 'NONE', #1050 ) ;
#2324 = CARTESIAN_POINT ( 'NONE',  ( 199.9999999999998863, 225.0000000000000284, 12.50000000000000000 ) ) ;
#2325 = VERTEX_POINT ( 'NONE', #6628 ) ;
#2326 = FACE_OUTER_BOUND ( 'NONE', #3099, .T. ) ;
#2327 = ORIENTED_EDGE ( 'NONE', *, *, #1299, .T. ) ;
#2328 = LINE ( 'NONE', #4762, #1508 ) ;
#2329 = DIRECTION ( 'NONE',  ( 0.000000000000000000, 0.000000000000000000, 1.000000000000000000 ) ) ;
#2330 = ORIENTED_EDGE ( 'NONE', *, *, #6604, .F. ) ;
#2331 = VERTEX_POINT ( 'NONE', #2338 ) ;
#2332 = EDGE_CURVE ( 'NONE', #1578, #3245, #5160, .T. ) ;
#2333 = VERTEX_POINT ( 'NONE', #459 ) ;
#2334 = ADVANCED_FACE ( 'NONE', ( #5343 ), #2305, .T. ) ;
#2335 = CARTESIAN_POINT ( 'NONE',  ( -6.495190528383286477, 16.25000000000000000, 7.500000000000000000 ) ) ;
#2336 = PLANE ( 'NONE',  #4849 ) ;
#2337 = DIRECTION ( 'NONE',  ( 0.000000000000000000, -1.000000000000000000, 0.000000000000000000 ) ) ;
#2338 = CARTESIAN_POINT ( 'NONE',  ( 12.50000000000000000, 3.827021247335477324E-15, -31.24999999999998579 ) ) ;
#2339 = CARTESIAN_POINT ( 'NONE',  ( 386.8189259714962986, 19.58130419088990948, -4.090982884146981746 ) ) ;
#2340 = EDGE_CURVE ( 'NONE', #6273, #1867, #2359, .T. ) ;
#2341 = VECTOR ( 'NONE', #7860, 1000.000000000000000 ) ;
#2342 = EDGE_CURVE ( 'NONE', #3094, #481, #1711, .T. ) ;
#2343 = CARTESIAN_POINT ( 'NONE',  ( 0.000000000000000000, 0.000000000000000000, 15.00000000000000000 ) ) ;
#2344 = FILL_AREA_STYLE_COLOUR ( '', #2918 ) ;
#2345 = DIRECTION ( 'NONE',  ( -1.000000000000000000, 0.000000000000000000, 0.000000000000000000 ) ) ;
#2346 = DIRECTION ( 'NONE',  ( 1.000000000000000000, 0.000000000000000000, 0.000000000000000000 ) ) ;
#2347 = FACE_OUTER_BOUND ( 'NONE', #520, .T. ) ;
#2348 = VERTEX_POINT ( 'NONE', #5587 ) ;
#2349 = EDGE_CURVE ( 'NONE', #994, #1161, #6744, .T. ) ;
#2350 = VERTEX_POINT ( 'NONE', #1887 ) ;
#2351 = DIRECTION ( 'NONE',  ( 1.000000000000000000, 0.000000000000000000, 0.000000000000000000 ) ) ;
#2352 = ORIENTED_EDGE ( 'NONE', *, *, #2919, .F. ) ;
#2353 = DIRECTION ( 'NONE',  ( 1.000000000000000000, 0.000000000000000000, 0.000000000000000000 ) ) ;
#2354 = CARTESIAN_POINT ( 'NONE',  ( 12.50000000000000000, 1.530808498934191521E-15, 75.00000000000000000 ) ) ;
#2355 = VERTEX_POINT ( 'NONE', #1291 ) ;
#2356 = DIRECTION ( 'NONE',  ( -1.000000000000000000, -0.000000000000000000, -0.000000000000000000 ) ) ;
#2357 = ORIENTED_EDGE ( 'NONE', *, *, #2144, .T. ) ;
#2358 = EDGE_CURVE ( 'NONE', #2323, #1867, #4294, .T. ) ;
#2359 = CIRCLE ( 'NONE', #3252, 25.00000000000000000 ) ;
#2360 = CYLINDRICAL_SURFACE ( 'NONE', #6268, 12.49999999999999822 ) ;
#2361 = ORIENTED_EDGE ( 'NONE', *, *, #980, .F. ) ;
#2362 = VECTOR ( 'NONE', #7716, 1000.000000000000000 ) ;
#2363 = CARTESIAN_POINT ( 'NONE',  ( 362.5007931252055187, -19.99950429724430023, 0.4454306286988182761 ) ) ;
#2364 = ORIENTED_EDGE ( 'NONE', *, *, #72, .T. ) ;
#2365 = FACE_OUTER_BOUND ( 'NONE', #4806, .T. ) ;
#2366 = AXIS2_PLACEMENT_3D ( 'NONE', #2670, #5108, #3796 ) ;
#2367 = ORIENTED_EDGE ( 'NONE', *, *, #5670, .F. ) ;
#2368 = EDGE_LOOP ( 'NONE', ( #1143, #6715, #3632, #3449 ) ) ;
#2369 = AXIS2_PLACEMENT_3D ( 'NONE', #5979, #6057, #4205 ) ;
#2370 = CARTESIAN_POINT ( 'NONE',  ( 379.1121327631079225, -16.14034269873396710, 11.81156333678811876 ) ) ;
#2371 = AXIS2_PLACEMENT_3D ( 'NONE', #4537, #4651, #1655 ) ;
#2372 = DIRECTION ( 'NONE',  ( -1.000000000000000000, -0.000000000000000000, -0.000000000000000000 ) ) ;
#2373 = LINE ( 'NONE', #7110, #6781 ) ;
#2374 = LINE ( 'NONE', #4130, #1222 ) ;
#2375 = DIRECTION ( 'NONE',  ( 0.000000000000000000, -1.000000000000000000, 0.000000000000000000 ) ) ;
#2376 = EDGE_CURVE ( 'NONE', #5001, #5902, #7732, .T. ) ;
#2377 = LINE ( 'NONE', #4814, #4801 ) ;
#2378 = AXIS2_PLACEMENT_3D ( 'NONE', #7670, #1536, #5909 ) ;
#2379 = CARTESIAN_POINT ( 'NONE',  ( 326.6025403784438481, 150.0000000000000568, 125.0000000000000000 ) ) ;
#2380 = DIRECTION ( 'NONE',  ( 4.789593822244094799E-16, 1.000000000000000000, 5.328524654824031087E-22 ) ) ;
#2381 = LINE ( 'NONE', #4818, #4691 ) ;
#2382 = CARTESIAN_POINT ( 'NONE',  ( 52.50000000000000711, 47.50000000000003553, 130.0000000000000000 ) ) ;
#2384 = DIRECTION ( 'NONE',  ( 1.000000000000000000, 0.000000000000000000, 0.000000000000000000 ) ) ;
#2383 = AXIS2_PLACEMENT_3D ( 'NONE', #2151, #4594, #2716 ) ;
#2385 = B_SPLINE_CURVE_WITH_KNOTS ( 'NONE', 3,
 ( #2224, #7837, #6674, #6635 ),
 .UNSPECIFIED., .F., .F.,
 ( 4, 4 ),
 ( 0.000000000000000000, 0.001270006434950044904 ),
 .UNSPECIFIED. ) ;
#2386 = DIRECTION ( 'NONE',  ( -1.000000000000000000, -2.960594732333750117E-15, 0.000000000000000000 ) ) ;
#2387 = VERTEX_POINT ( 'NONE', #2005 ) ;
#2388 = ADVANCED_FACE ( 'NONE', ( #3817 ), #202, .T. ) ;
#2389 = ADVANCED_FACE ( 'NONE', ( #2653 ), #1407, .F. ) ;
#2390 = ORIENTED_EDGE ( 'NONE', *, *, #7251, .F. ) ;
#2391 = CIRCLE ( 'NONE', #5848, 25.00000000000000000 ) ;
#2392 = VERTEX_POINT ( 'NONE', #162 ) ;
#2393 = DIRECTION ( 'NONE',  ( 1.000000000000000000, 0.000000000000000000, -0.000000000000000000 ) ) ;
#2394 = CARTESIAN_POINT ( 'NONE',  ( 4.000000000000004441, 0.000000000000000000, 35.78244274809159720 ) ) ;
#2395 = FILL_AREA_STYLE_COLOUR ( '', #4663 ) ;
#2396 = ORIENTED_EDGE ( 'NONE', *, *, #3311, .F. ) ;
#2397 = AXIS2_PLACEMENT_3D ( 'NONE', #5953, #7799, #7237 ) ;
#2398 = CARTESIAN_POINT ( 'NONE',  ( 12.50000000000000000, 24.99999999999999645, 37.50000000000000711 ) ) ;
#2399 = ORIENTED_EDGE ( 'NONE', *, *, #3554, .T. ) ;
#2400 = CIRCLE ( 'NONE', #3551, 65.50000000000000000 ) ;
#2401 = LINE ( 'NONE', #521, #1020 ) ;
#2402 = ORIENTED_EDGE ( 'NONE', *, *, #5255, .T. ) ;
#2403 = DIRECTION ( 'NONE',  ( 0.000000000000000000, 0.000000000000000000, -1.000000000000000000 ) ) ;
#2404 = ORIENTED_EDGE ( 'NONE', *, *, #2858, .T. ) ;
#2405 = CARTESIAN_POINT ( 'NONE',  ( 412.5000000000001137, 217.5000000000000000, 20.00000000000000000 ) ) ;
#2406 = DIRECTION ( 'NONE',  ( 1.000000000000000000, 0.000000000000000000, 0.000000000000000000 ) ) ;
#2407 = EDGE_CURVE ( 'NONE', #3577, #3835, #2752, .T. ) ;
#2408 = VECTOR ( 'NONE', #1841, 1000.000000000000000 ) ;
#2409 = ORIENTED_EDGE ( 'NONE', *, *, #7191, .T. ) ;
#2410 = ORIENTED_EDGE ( 'NONE', *, *, #2491, .F. ) ;
#2411 = VECTOR ( 'NONE', #1682, 1000.000000000000000 ) ;
#2412 = CIRCLE ( 'NONE', #2936, 15.64999999999999680 ) ;
#2413 = CARTESIAN_POINT ( 'NONE',  ( 377.0997413288390021, -15.74791738283697740, 12.32940567573685087 ) ) ;
#2414 = LINE ( 'NONE', #7192, #2135 ) ;
#2415 = CARTESIAN_POINT ( 'NONE',  ( 1.320471425210250835E-15, 0.000000000000000000, 0.000000000000000000 ) ) ;
#2416 = CARTESIAN_POINT ( 'NONE',  ( 398.0000000000001137, 12.50000000000000000, 15.61249499599599488 ) ) ;
#2417 = LINE ( 'NONE', #5384, #574 ) ;
#2418 = CARTESIAN_POINT ( 'NONE',  ( 375.0000000000000000, 15.61249499599599488, -12.50000000000000000 ) ) ;
#2419 = CIRCLE ( 'NONE', #1522, 5.000000000000004441 ) ;
#2420 = CARTESIAN_POINT ( 'NONE',  ( -6.495190528383282036, -16.24999999999999645, 0.000000000000000000 ) ) ;
#2421 = SHAPE_DEFINITION_REPRESENTATION ( #4492, #4527 ) ;
#2422 = EDGE_CURVE ( 'NONE', #1166, #1544, #3217, .T. ) ;
#2423 = VECTOR ( 'NONE', #5152, 1000.000000000000000 ) ;
#2424 = DIRECTION ( 'NONE',  ( 0.000000000000000000, 0.000000000000000000, 1.000000000000000000 ) ) ;
#2425 = LINE ( 'NONE', #6791, #2156 ) ;
#2426 = AXIS2_PLACEMENT_3D ( 'NONE', #4366, #6146, #7429 ) ;
#2427 = LINE ( 'NONE', #5593, #828 ) ;
#2428 = LINE ( 'NONE', #5996, #4030 ) ;
#2429 = ORIENTED_EDGE ( 'NONE', *, *, #1309, .T. ) ;
#2430 = ADVANCED_FACE ( 'NONE', ( #1251 ), #1588, .T. ) ;
#2431 = ORIENTED_EDGE ( 'NONE', *, *, #3311, .T. ) ;
#2432 = CARTESIAN_POINT ( 'NONE',  ( 0.000000000000000000, 0.000000000000000000, 25.00000000000000000 ) ) ;
#2433 = CARTESIAN_POINT ( 'NONE',  ( 6.495190528383289141, -11.24999999999999645, 7.500000000000000000 ) ) ;
#2434 = DIRECTION ( 'NONE',  ( 1.000000000000000000, 0.000000000000000000, 0.000000000000000000 ) ) ;
#2435 = EDGE_CURVE ( 'NONE', #5563, #6259, #6226, .T. ) ;
#2436 = CARTESIAN_POINT ( 'NONE',  ( 212.4999999999999147, 225.0000000000000284, 12.50000000000000000 ) ) ;
#2437 = ORIENTED_EDGE ( 'NONE', *, *, #2675, .T. ) ;
#2438 = CARTESIAN_POINT ( 'NONE',  ( 41.25000000000002842, 0.000000000000000000, 17.50000000000000000 ) ) ;
#2439 = ADVANCED_FACE ( 'NONE', ( #4935 ), #5090, .T. ) ;
#2440 = ORIENTED_EDGE ( 'NONE', *, *, #1008, .F. ) ;
#2441 = CARTESIAN_POINT ( 'NONE',  ( 362.4991219212881788, 20.00054879841449562, 0.3963588355767777571 ) ) ;
#2442 = ORIENTED_EDGE ( 'NONE', *, *, #3393, .F. ) ;
#2443 = DIRECTION ( 'NONE',  ( 1.000000000000000000, 0.000000000000000000, -0.000000000000000000 ) ) ;
#2444 = ORIENTED_EDGE ( 'NONE', *, *, #3470, .F. ) ;
#2445 =( LENGTH_UNIT ( ) NAMED_UNIT ( * ) SI_UNIT ( .MILLI., .METRE. ) );
#2446 = LINE ( 'NONE', #3845, #824 ) ;
#2447 =( GEOMETRIC_REPRESENTATION_CONTEXT ( 3 ) GLOBAL_UNCERTAINTY_ASSIGNED_CONTEXT ( ( #2473 ) ) GLOBAL_UNIT_ASSIGNED_CONTEXT ( ( #2506, #3678, #5515 ) ) REPRESENTATION_CONTEXT ( 'NONE', 'WORKASPACE' ) );
#2448 = ORIENTED_EDGE ( 'NONE', *, *, #5214, .T. ) ;
#2449 = AXIS2_PLACEMENT_3D ( 'NONE', #5987, #7111, #3501 ) ;
#2450 = EDGE_LOOP ( 'NONE', ( #7615, #3602, #5433, #1388 ) ) ;
#2451 = ORIENTED_EDGE ( 'NONE', *, *, #1464, .F. ) ;
#2452 = FACE_BOUND ( 'NONE', #4509, .T. ) ;
#2453 = DIRECTION ( 'NONE',  ( 1.000000000000000000, 0.000000000000000000, 0.000000000000000000 ) ) ;
#2454 = DIRECTION ( 'NONE',  ( -0.000000000000000000, 0.000000000000000000, 1.000000000000000000 ) ) ;
#2455 = CARTESIAN_POINT ( 'NONE',  ( 41.25000000000002842, 177.6587708172407076, 12.50000000000000000 ) ) ;
#2456 = AXIS2_PLACEMENT_3D ( 'NONE', #1134, #4740, #6472 ) ;
#2457 = PLANE ( 'NONE',  #3771 ) ;
#2458 = CARTESIAN_POINT ( 'NONE',  ( 387.4765783011941380, 19.98534102192048323, 0.8725863811532602599 ) ) ;
#2459 = ADVANCED_FACE ( 'NONE', ( #685 ), #5704, .T. ) ;
#2460 = DIRECTION ( 'NONE',  ( -0.5000000000000000000, -0.8660254037844385966, 0.000000000000000000 ) ) ;
#2461 = ITEM_DEFINED_TRANSFORMATION ( 'NONE', 'NONE', #3747,  #5785 ) ;
#2462 = DIRECTION ( 'NONE',  ( 0.000000000000000000, 1.000000000000000000, 0.000000000000000000 ) ) ;
#2463 = LINE ( 'NONE', #3788, #185 ) ;
#2464 = CARTESIAN_POINT ( 'NONE',  ( -0.000000000000000000, 187.4999999999999432, 0.000000000000000000 ) ) ;
#2465 = ORIENTED_EDGE ( 'NONE', *, *, #6346, .F. ) ;
#2466 = SHAPE_REPRESENTATION_RELATIONSHIP ( 'NONE' , 'NONE' ,  #6180, #676 ) ;
#2467 = ORIENTED_EDGE ( 'NONE', *, *, #4772, .T. ) ;
#2468 = DIRECTION ( 'NONE',  ( 1.000000000000000000, 0.000000000000000000, 0.000000000000000000 ) ) ;
#2469 = CARTESIAN_POINT ( 'NONE',  ( 340.0000000000000000, 12.50000000000000000, -15.61249499599599488 ) ) ;
#2470 =( NAMED_UNIT ( * ) PLANE_ANGLE_UNIT ( ) SI_UNIT ( $, .RADIAN. ) );
#2471 = ORIENTED_EDGE ( 'NONE', *, *, #7535, .T. ) ;
#2472 = DIRECTION ( 'NONE',  ( 1.000000000000000000, 0.000000000000000000, 0.000000000000000000 ) ) ;
#2473 = UNCERTAINTY_MEASURE_WITH_UNIT (LENGTH_MEASURE( 1.000000000000000082E-05 ), #2506, 'distance_accuracy_value', 'NONE');
#2474 = ADVANCED_FACE ( 'NONE', ( #1365 ), #125, .F. ) ;
#2475 = ORIENTED_EDGE ( 'NONE', *, *, #2928, .T. ) ;
#2476 = CARTESIAN_POINT ( 'NONE',  ( 368.6894672773787534, 16.82862359362766469, -10.81999899256329911 ) ) ;
#2477 = VERTEX_POINT ( 'NONE', #1326 ) ;
#2478 = CARTESIAN_POINT ( 'NONE',  ( 365.1180127946531115, -18.47584224143657039, 7.665216593424116986 ) ) ;
#2479 = ORIENTED_EDGE ( 'NONE', *, *, #6468, .T. ) ;
#2480 = CLOSED_SHELL ( 'NONE', ( #3764, #7533, #7385, #6698, #3262, #1391, #7578, #1058, #5019, #1395, #2430 ) ) ;
#2481 = FACE_OUTER_BOUND ( 'NONE', #2368, .T. ) ;
#2482 = EDGE_CURVE ( 'NONE', #243, #3363, #7609, .T. ) ;
#2483 = CARTESIAN_POINT ( 'NONE',  ( 0.000000000000000000, 0.000000000000000000, 0.000000000000000000 ) ) ;
#2484 = EDGE_CURVE ( 'NONE', #7797, #5801, #1959, .T. ) ;
#2485 = EDGE_CURVE ( 'NONE', #4115, #4623, #5047, .T. ) ;
#2486 = ORIENTED_EDGE ( 'NONE', *, *, #3414, .T. ) ;
#2487 = AXIS2_PLACEMENT_3D ( 'NONE', #553, #5482, #2282 ) ;
#2488 = ORIENTED_EDGE ( 'NONE', *, *, #820, .T. ) ;
#2489 = ORIENTED_EDGE ( 'NONE', *, *, #3807, .F. ) ;
#2490 = CYLINDRICAL_SURFACE ( 'NONE', #226, 4.999999999999997335 ) ;
#2491 = EDGE_CURVE ( 'NONE', #6165, #3100, #5823, .T. ) ;
#2492 = CARTESIAN_POINT ( 'NONE',  ( 387.3337822858457002, -19.89643035834168927, 2.074044983930025232 ) ) ;
#2493 = DIRECTION ( 'NONE',  ( 1.000000000000000000, 0.000000000000000000, 0.000000000000000000 ) ) ;
#2494 = DIRECTION ( 'NONE',  ( 0.000000000000000000, 0.000000000000000000, -1.000000000000000000 ) ) ;
#2495 = VECTOR ( 'NONE', #7655, 1000.000000000000000 ) ;
#2496 = CARTESIAN_POINT ( 'NONE',  ( 62.50000000000007105, 79.24999999999987210, 130.0000000000000000 ) ) ;
#2497 = AXIS2_PLACEMENT_3D ( 'NONE', #142, #220, #2588 ) ;
#2498 = EDGE_CURVE ( 'NONE', #6738, #784, #2047, .T. ) ;
#2499 = FACE_OUTER_BOUND ( 'NONE', #5406, .T. ) ;
#2500 = CARTESIAN_POINT ( 'NONE',  ( -37.49999999999995026, 37.50000000000010658, 12.50000000000000000 ) ) ;
#2501 = CARTESIAN_POINT ( 'NONE',  ( 0.000000000000000000, 0.000000000000000000, 0.000000000000000000 ) ) ;
#2502 = CARTESIAN_POINT ( 'NONE',  ( 50.71904415029504065, 62.70544120911855401, 12.50000000000000000 ) ) ;
#2503 = AXIS2_PLACEMENT_3D ( 'NONE', #6704, #3622, #4133 ) ;
#2504 = ADVANCED_FACE ( 'NONE', ( #7100 ), #2730, .F. ) ;
#2505 = VERTEX_POINT ( 'NONE', #7701 ) ;
#2506 =( LENGTH_UNIT ( ) NAMED_UNIT ( * ) SI_UNIT ( .MILLI., .METRE. ) );
#2507 = EDGE_LOOP ( 'NONE', ( #6851, #1156, #568, #3769, #4549 ) ) ;
#2508 = DIRECTION ( 'NONE',  ( -0.8660254037844384856, -0.5000000000000004441, 0.000000000000000000 ) ) ;
#2509 = DIRECTION ( 'NONE',  ( -1.000000000000000000, 0.000000000000000000, 0.000000000000000000 ) ) ;
#2510 = CARTESIAN_POINT ( 'NONE',  ( 400.0000000000000568, -25.00000000000000000, 25.00000000000000000 ) ) ;
#2511 = LINE ( 'NONE', #4951, #944 ) ;
#2512 = EDGE_LOOP ( 'NONE', ( #1625, #240, #6975, #5598, #67 ) ) ;
#2513 = LINE ( 'NONE', #4954, #3790 ) ;
#2514 = AXIS2_PLACEMENT_3D ( 'NONE', #1548, #2110, #1512 ) ;
#2515 = ORIENTED_EDGE ( 'NONE', *, *, #6411, .F. ) ;
#2516 = CARTESIAN_POINT ( 'NONE',  ( 365.6127344411505646, 18.21073727249144625, 8.292169370763099678 ) ) ;
#2517 = VERTEX_POINT ( 'NONE', #1005 ) ;
#2518 = LINE ( 'NONE', #868, #7125 ) ;
#2519 = AXIS2_PLACEMENT_3D ( 'NONE', #129, #4451, #3148 ) ;
#2520 = ORIENTED_EDGE ( 'NONE', *, *, #5693, .T. ) ;
#2521 = DIRECTION ( 'NONE',  ( 1.000000000000000000, 0.000000000000000000, 0.000000000000000000 ) ) ;
#2522 = FACE_OUTER_BOUND ( 'NONE', #2200, .T. ) ;
#2523 = VECTOR ( 'NONE', #3819, 1000.000000000000000 ) ;
#2524 = ORIENTED_EDGE ( 'NONE', *, *, #2422, .F. ) ;
#2525 = ORIENTED_EDGE ( 'NONE', *, *, #4737, .T. ) ;
#2526 = EDGE_CURVE ( 'NONE', #1390, #1064, #4914, .T. ) ;
#2527 = VERTEX_POINT ( 'NONE', #2209 ) ;
#2528 = CARTESIAN_POINT ( 'NONE',  ( 412.4999999999998295, 150.0000000000000284, 5.000000000000000000 ) ) ;
#2529 = CARTESIAN_POINT ( 'NONE',  ( -25.00000000000000000, 24.99999999999999289, 50.00000000000000000 ) ) ;
#2530 = CARTESIAN_POINT ( 'NONE',  ( 12.50000000000000355, 0.000000000000000000, 77.49999999999998579 ) ) ;
#2532 = CARTESIAN_POINT ( 'NONE',  ( 50.71904415029504065, 87.70544117646394966, 12.50000000000000000 ) ) ;
#2531 = AXIS2_PLACEMENT_3D ( 'NONE', #880, #281, #840 ) ;
#2533 = EDGE_CURVE ( 'NONE', #2900, #6485, #1439, .T. ) ;
#2534 = DIRECTION ( 'NONE',  ( -0.000000000000000000, -0.000000000000000000, -1.000000000000000000 ) ) ;
#2535 = AXIS2_PLACEMENT_3D ( 'NONE', #6456, #2252, #7061 ) ;
#2536 = VECTOR ( 'NONE', #2165, 1000.000000000000000 ) ;
#2537 = SHAPE_DEFINITION_REPRESENTATION ( #409, #444 ) ;
#2538 = PLANE ( 'NONE',  #3044 ) ;
#2539 = CARTESIAN_POINT ( 'NONE',  ( 5.204170427930428856E-14, 37.50000000000005684, 12.50000000000000000 ) ) ;
#2540 = DIRECTION ( 'NONE',  ( 0.000000000000000000, 0.000000000000000000, 1.000000000000000000 ) ) ;
#2541 = DIRECTION ( 'NONE',  ( -0.000000000000000000, 0.000000000000000000, 1.000000000000000000 ) ) ;
#2542 = CIRCLE ( 'NONE', #241, 12.50000000000000355 ) ;
#2543 = VECTOR ( 'NONE', #7633, 1000.000000000000000 ) ;
#2544 = EDGE_LOOP ( 'NONE', ( #6663, #1556 ) ) ;
#2545 = AXIS2_PLACEMENT_3D ( 'NONE', #4773, #1053, #5217 ) ;
#2546 = AXIS2_PLACEMENT_3D ( 'NONE', #422, #2312, #2345 ) ;
#2547 = ORIENTED_EDGE ( 'NONE', *, *, #4245, .F. ) ;
#2548 = EDGE_CURVE ( 'NONE', #5801, #1936, #5300, .T. ) ;
#2549 = DIRECTION ( 'NONE',  ( 1.000000000000000000, 0.000000000000000000, 0.000000000000000000 ) ) ;
#2550 = CARTESIAN_POINT ( 'NONE',  ( 150.0000000000000000, 1.836970198721029747E-14, 25.00000000000000000 ) ) ;
#2551 = DIRECTION ( 'NONE',  ( 1.000000000000000000, 0.000000000000000000, 0.000000000000000000 ) ) ;
#2552 = ORIENTED_EDGE ( 'NONE', *, *, #2297, .T. ) ;
#2553 = CARTESIAN_POINT ( 'NONE',  ( 41.25000000000002842, 177.5000000000000000, 17.50000000000000000 ) ) ;
#2554 = CIRCLE ( 'NONE', #7036, 20.00000000000000000 ) ;
#2555 = VECTOR ( 'NONE', #6582, 1000.000000000000227 ) ;
#2556 = UNCERTAINTY_MEASURE_WITH_UNIT (LENGTH_MEASURE( 1.000000000000000082E-05 ), #2962, 'distance_accuracy_value', 'NONE');
#2557 = ORIENTED_EDGE ( 'NONE', *, *, #3197, .T. ) ;
#2558 = CARTESIAN_POINT ( 'NONE',  ( 362.9438371151090905, 19.72539574521466932, -3.327763323014857555 ) ) ;
#2559 = EDGE_LOOP ( 'NONE', ( #2357, #5062, #1264, #65, #5031, #2488, #6544, #1359, #5456, #3854 ) ) ;
#2560 = CARTESIAN_POINT ( 'NONE',  ( 375.0000000000000000, 25.00000000000000000, 3.061616997868383043E-15 ) ) ;
#2561 = ORIENTED_EDGE ( 'NONE', *, *, #4980, .F. ) ;
#2562 = CARTESIAN_POINT ( 'NONE',  ( 62.50000000000008527, 111.9999999999998863, 130.0000000000000000 ) ) ;
#2563 = DIRECTION ( 'NONE',  ( -0.000000000000000000, -0.000000000000000000, -1.000000000000000000 ) ) ;
#2564 = ORIENTED_EDGE ( 'NONE', *, *, #4771, .F. ) ;
#2565 = VERTEX_POINT ( 'NONE', #363 ) ;
#2566 = ORIENTED_EDGE ( 'NONE', *, *, #4482, .F. ) ;
#2567 = DIRECTION ( 'NONE',  ( 0.000000000000000000, 0.000000000000000000, 1.000000000000000000 ) ) ;
#2568 = CARTESIAN_POINT ( 'NONE',  ( 377.9017428551080116, -15.87479745381989815, -12.16559770555248754 ) ) ;
#2569 = CARTESIAN_POINT ( 'NONE',  ( 286.6025403784439050, 0.000000000000000000, 0.000000000000000000 ) ) ;
#2570 = ORIENTED_EDGE ( 'NONE', *, *, #7730, .T. ) ;
#2571 = DIRECTION ( 'NONE',  ( -0.000000000000000000, -0.000000000000000000, 1.000000000000000000 ) ) ;
#2572 = ADVANCED_FACE ( 'NONE', ( #4643 ), #2122, .F. ) ;
#2573 = EDGE_CURVE ( 'NONE', #2057, #6240, #950, .T. ) ;
#2574 = PRODUCT ( 'Nut', 'Nut', '', ( #5387 ) ) ;
#2575 = CIRCLE ( 'NONE', #7694, 12.49999999999999822 ) ;
#2576 = CARTESIAN_POINT ( 'NONE',  ( 400.0000000000000000, -12.50000000000000000, 25.00000000000000000 ) ) ;
#2577 = FACE_OUTER_BOUND ( 'NONE', #5442, .T. ) ;
#2578 = CARTESIAN_POINT ( 'NONE',  ( 0.000000000000000000, 0.000000000000000000, 7.500000000000000000 ) ) ;
#2579 = CYLINDRICAL_SURFACE ( 'NONE', #5051, 12.50000000000000000 ) ;
#2580 = EDGE_CURVE ( 'NONE', #3479, #3721, #1081, .T. ) ;
#2581 = EDGE_CURVE ( 'NONE', #2355, #2843, #6378, .T. ) ;
#2582 = PRODUCT_DEFINITION_FORMATION_WITH_SPECIFIED_SOURCE ( 'ANY', '', #2127, .NOT_KNOWN. ) ;
#2583 = ORIENTED_EDGE ( 'NONE', *, *, #7191, .F. ) ;
#2584 =( LENGTH_UNIT ( ) NAMED_UNIT ( * ) SI_UNIT ( .MILLI., .METRE. ) );
#2585 = VERTEX_POINT ( 'NONE', #3293 ) ;
#2586 = CARTESIAN_POINT ( 'NONE',  ( 10.82531754730547213, 13.75000000000000178, 0.000000000000000000 ) ) ;
#2587 = CYLINDRICAL_SURFACE ( 'NONE', #7104, 5.000000000000000000 ) ;
#2588 = DIRECTION ( 'NONE',  ( 0.000000000000000000, 0.000000000000000000, 1.000000000000000000 ) ) ;
#2589 = EDGE_LOOP ( 'NONE', ( #138, #6963 ) ) ;
#2590 = CARTESIAN_POINT ( 'NONE',  ( -25.00000000000000711, 0.000000000000000000, 25.00000000000000000 ) ) ;
#2591 = APPLICATION_CONTEXT ( 'automotive_design' ) ;
#2592 = ORIENTED_EDGE ( 'NONE', *, *, #273, .F. ) ;
#2593 = VECTOR ( 'NONE', #4215, 1000.000000000000000 ) ;
#2594 = DIRECTION ( 'NONE',  ( 0.000000000000000000, 0.000000000000000000, 1.000000000000000000 ) ) ;
#2595 = ORIENTED_EDGE ( 'NONE', *, *, #4875, .F. ) ;
#2596 = DIRECTION ( 'NONE',  ( -0.000000000000000000, -0.000000000000000000, -1.000000000000000000 ) ) ;
#2597 = ORIENTED_EDGE ( 'NONE', *, *, #1367, .T. ) ;
#2598 = DIRECTION ( 'NONE',  ( 1.000000000000000000, 0.000000000000000000, 0.000000000000000000 ) ) ;
#2599 = CARTESIAN_POINT ( 'NONE',  ( -37.49999999999990763, 144.7499999999999432, 130.0000000000000000 ) ) ;
#2600 = EDGE_CURVE ( 'NONE', #260, #4272, #4489, .T. ) ;
#2601 = VERTEX_POINT ( 'NONE', #6419 ) ;
#2602 = CARTESIAN_POINT ( 'NONE',  ( 286.6025403784437913, 135.0000000000000000, 0.000000000000000000 ) ) ;
#2603 = ORIENTED_EDGE ( 'NONE', *, *, #7440, .T. ) ;
#2604 = ORIENTED_EDGE ( 'NONE', *, *, #5227, .T. ) ;
#2605 = CARTESIAN_POINT ( 'NONE',  ( 375.0000000000000000, 25.00000000000000000, 3.061616997868383043E-15 ) ) ;
#2606 = CARTESIAN_POINT ( 'NONE',  ( 383.2551259162264614, -17.65381669312412427, -9.419798908014916705 ) ) ;
#2607 = ORIENTED_EDGE ( 'NONE', *, *, #7682, .T. ) ;
#2608 = DIRECTION ( 'NONE',  ( -1.000000000000000000, 0.000000000000000000, 0.000000000000000000 ) ) ;
#2609 = AXIS2_PLACEMENT_3D ( 'NONE', #3863, #2013, #3789 ) ;
#2610 = VECTOR ( 'NONE', #1609, 1000.000000000000000 ) ;
#2611 = VECTOR ( 'NONE', #3909, 1000.000000000000000 ) ;
#2612 = PRODUCT_RELATED_PRODUCT_CATEGORY ( 'part', '', ( #2574 ) ) ;
#2613 = FACE_OUTER_BOUND ( 'NONE', #894, .T. ) ;
#2614 = CARTESIAN_POINT ( 'NONE',  ( 42.50000000000000000, 42.50000000000003553, 12.50000000000000000 ) ) ;
#2615 = DIRECTION ( 'NONE',  ( -0.000000000000000000, -0.000000000000000000, -1.000000000000000000 ) ) ;
#2616 = CARTESIAN_POINT ( 'NONE',  ( -36.78095584970496645, 12.70544120911856290, 0.000000000000000000 ) ) ;
#2617 = AXIS2_PLACEMENT_3D ( 'NONE', #3183, #2571, #5014 ) ;
#2618 = PRESENTATION_LAYER_ASSIGNMENT (  '', '', ( #6085 ) ) ;
#2619 = VECTOR ( 'NONE', #165, 1000.000000000000000 ) ;
#2620 = EDGE_LOOP ( 'NONE', ( #5513, #2240, #835, #3415 ) ) ;
#2621 = FACE_OUTER_BOUND ( 'NONE', #3613, .T. ) ;
#2622 = ORIENTED_EDGE ( 'NONE', *, *, #4401, .F. ) ;
#2623 = EDGE_CURVE ( 'NONE', #3835, #6817, #2880, .T. ) ;
#2624 = DIRECTION ( 'NONE',  ( -1.000000000000000000, 0.000000000000000000, 0.000000000000000000 ) ) ;
#2626 = CARTESIAN_POINT ( 'NONE',  ( 47.36967921662626679, 6.904171036223937463, 12.50000000000000000 ) ) ;
#2625 = VECTOR ( 'NONE', #7381, 1000.000000000000000 ) ;
#2627 = AXIS2_PLACEMENT_3D ( 'NONE', #4572, #5211, #415 ) ;
#2628 = AXIS2_PLACEMENT_3D ( 'NONE', #2012, #4453, #5210 ) ;
#2629 = DIRECTION ( 'NONE',  ( 0.000000000000000000, 0.000000000000000000, -1.000000000000000000 ) ) ;
#2630 = ORIENTED_EDGE ( 'NONE', *, *, #236, .F. ) ;
#2631 = ADVANCED_FACE ( 'NONE', ( #3371 ), #5744, .F. ) ;
#2632 = AXIS2_PLACEMENT_3D ( 'NONE', #2553, #1943, #6167 ) ;
#2633 = ORIENTED_EDGE ( 'NONE', *, *, #3755, .F. ) ;
#2634 = ADVANCED_FACE ( 'NONE', ( #6982, #1482 ), #320, .F. ) ;
#2635 = EDGE_CURVE ( 'NONE', #387, #389, #5438, .T. ) ;
#2636 = FACE_BOUND ( 'NONE', #2859, .T. ) ;
#2637 = VERTEX_POINT ( 'NONE', #7658 ) ;
#2638 = CARTESIAN_POINT ( 'NONE',  ( 150.0000000000000000, 1.836970198721029747E-14, 0.000000000000000000 ) ) ;
#2639 = ORIENTED_EDGE ( 'NONE', *, *, #5542, .F. ) ;
#2640 = FACE_OUTER_BOUND ( 'NONE', #1758, .T. ) ;
#2641 = AXIS2_PLACEMENT_3D ( 'NONE', #5896, #1076, #400 ) ;
#2642 = CARTESIAN_POINT ( 'NONE',  ( 296.6025403784439050, 90.00000000000001421, 12.50000000000000000 ) ) ;
#2643 = VERTEX_POINT ( 'NONE', #4006 ) ;
#2644 = VECTOR ( 'NONE', #5436, 1000.000000000000000 ) ;
#2645 = CARTESIAN_POINT ( 'NONE',  ( 296.6025403784439050, 0.000000000000000000, 12.50000000000000000 ) ) ;
#2646 = ORIENTED_EDGE ( 'NONE', *, *, #291, .F. ) ;
#2647 = ORIENTED_EDGE ( 'NONE', *, *, #1651, .F. ) ;
#2648 = DIRECTION ( 'NONE',  ( 0.000000000000000000, -0.000000000000000000, 1.000000000000000000 ) ) ;
#2649 = EDGE_CURVE ( 'NONE', #2853, #5178, #6457, .T. ) ;
#2650 = FACE_OUTER_BOUND ( 'NONE', #680, .T. ) ;
#2651 = CARTESIAN_POINT ( 'NONE',  ( 325.0000000000000000, 3.061616997868383043E-15, -25.00000000000000000 ) ) ;
#2652 = ORIENTED_EDGE ( 'NONE', *, *, #4929, .F. ) ;
#2653 = FACE_OUTER_BOUND ( 'NONE', #3966, .T. ) ;
#2654 = AXIS2_PLACEMENT_3D ( 'NONE', #6633, #2424, #542 ) ;
#2655 = ADVANCED_FACE ( 'NONE', ( #2365 ), #7187, .F. ) ;
#2656 = DIRECTION ( 'NONE',  ( -0.000000000000000000, -0.000000000000000000, -1.000000000000000000 ) ) ;
#2657 = PLANE ( 'NONE',  #6011 ) ;
#2658 = DIRECTION ( 'NONE',  ( 1.000000000000000000, 0.000000000000000000, 0.000000000000000000 ) ) ;
#2659 = DIRECTION ( 'NONE',  ( 0.000000000000000000, -1.000000000000000000, 0.000000000000000000 ) ) ;
#2660 = AXIS2_PLACEMENT_3D ( 'NONE', #7289, #6083, #4189 ) ;
#2661 = EDGE_LOOP ( 'NONE', ( #407, #7170, #5918, #2029 ) ) ;
#2662 = DIRECTION ( 'NONE',  ( -0.000000000000000000, -0.000000000000000000, -1.000000000000000000 ) ) ;
#2663 = CARTESIAN_POINT ( 'NONE',  ( -375.9131605378006498, 164.1990734970207768, 183.2402661832477122 ) ) ;
#2664 = ORIENTED_EDGE ( 'NONE', *, *, #3323, .T. ) ;
#2665 = VECTOR ( 'NONE', #7419, 1000.000000000000000 ) ;
#2666 = DIRECTION ( 'NONE',  ( 0.8660254037844387076, -0.5000000000000001110, 0.000000000000000000 ) ) ;
#2667 = DIRECTION ( 'NONE',  ( -1.000000000000000000, 0.000000000000000000, 0.000000000000000000 ) ) ;
#2668 = VECTOR ( 'NONE', #5915, 1000.000000000000000 ) ;
#2669 = DIRECTION ( 'NONE',  ( -0.000000000000000000, 0.000000000000000000, -1.000000000000000000 ) ) ;
#2670 = CARTESIAN_POINT ( 'NONE',  ( -49.28095584970496645, 12.70544120911856112, 12.50000000000000000 ) ) ;
#2671 = ORIENTED_EDGE ( 'NONE', *, *, #4811, .F. ) ;
#2672 =( GEOMETRIC_REPRESENTATION_CONTEXT ( 3 ) GLOBAL_UNCERTAINTY_ASSIGNED_CONTEXT ( ( #5606 ) ) GLOBAL_UNIT_ASSIGNED_CONTEXT ( ( #4459, #4541, #5022 ) ) REPRESENTATION_CONTEXT ( 'NONE', 'WORKASPACE' ) );
#2673 = EDGE_CURVE ( 'NONE', #2860, #4784, #4788, .T. ) ;
#2674 = ORIENTED_EDGE ( 'NONE', *, *, #7522, .T. ) ;
#2675 = EDGE_CURVE ( 'NONE', #646, #5119, #1079, .T. ) ;
#2676 = CARTESIAN_POINT ( 'NONE',  ( 175.0000000000000000, 0.000000000000000000, 0.000000000000000000 ) ) ;
#2677 = ORIENTED_EDGE ( 'NONE', *, *, #1408, .T. ) ;
#2678 = DIRECTION ( 'NONE',  ( -0.000000000000000000, -0.000000000000000000, -1.000000000000000000 ) ) ;
#2679 = CARTESIAN_POINT ( 'NONE',  ( 46.25000000000002842, 0.000000000000000000, 195.5000000000000000 ) ) ;
#2680 = VECTOR ( 'NONE', #2460, 1000.000000000000227 ) ;
#2681 = DIRECTION ( 'NONE',  ( 0.000000000000000000, -0.000000000000000000, -1.000000000000000000 ) ) ;
#2682 = AXIS2_PLACEMENT_3D ( 'NONE', #7348, #2493, #4974 ) ;
#2683 = ADVANCED_BREP_SHAPE_REPRESENTATION ( '', ( #7024, #5785 ), #2702 ) ;
#2684 = CARTESIAN_POINT ( 'NONE',  ( 3.592258498106024636E-14, 75.00000000000019895, 12.50000000000000000 ) ) ;
#2685 = EDGE_CURVE ( 'NONE', #136, #2585, #6461, .T. ) ;
#2686 = ORIENTED_EDGE ( 'NONE', *, *, #7323, .F. ) ;
#2687 = DIRECTION ( 'NONE',  ( -1.000000000000000000, 0.000000000000000000, 0.000000000000000000 ) ) ;
#2688 = ORIENTED_EDGE ( 'NONE', *, *, #3226, .F. ) ;
#2689 = ORIENTED_EDGE ( 'NONE', *, *, #4334, .T. ) ;
#2690 = CARTESIAN_POINT ( 'NONE',  ( 340.0000000000000000, -12.50000000000000355, 0.000000000000000000 ) ) ;
#2691 = CARTESIAN_POINT ( 'NONE',  ( -10.82531754730547924, 13.75000000000000000, 7.500000000000000000 ) ) ;
#2692 = DIRECTION ( 'NONE',  ( -2.960594732333750117E-15, 1.000000000000000000, 0.000000000000000000 ) ) ;
#2693 = DIRECTION ( 'NONE',  ( -0.000000000000000000, 0.000000000000000000, 1.000000000000000000 ) ) ;
#2694 = ORIENTED_EDGE ( 'NONE', *, *, #1911, .F. ) ;
#2695 = CARTESIAN_POINT ( 'NONE',  ( 296.6025403784437913, 137.4999999999999716, 12.50000000000000000 ) ) ;
#2696 = CARTESIAN_POINT ( 'NONE',  ( -37.49999999999992184, 111.9999999999999289, 130.0000000000000000 ) ) ;
#2697 = CARTESIAN_POINT ( 'NONE',  ( 11.46392929283375928, -22.21662272193747256, 25.00000000000000000 ) ) ;
#2698 = DIRECTION ( 'NONE',  ( 0.000000000000000000, 0.000000000000000000, -1.000000000000000000 ) ) ;
#2699 =( REPRESENTATION_RELATIONSHIP ('NONE','NONE', #6292, #949 ) REPRESENTATION_RELATIONSHIP_WITH_TRANSFORMATION ( #3031 )SHAPE_REPRESENTATION_RELATIONSHIP( ) );
#2700 = ADVANCED_FACE ( 'NONE', ( #6099 ), #2296, .T. ) ;
#2701 = ORIENTED_EDGE ( 'NONE', *, *, #1322, .T. ) ;
#2702 =( GEOMETRIC_REPRESENTATION_CONTEXT ( 3 ) GLOBAL_UNCERTAINTY_ASSIGNED_CONTEXT ( ( #937 ) ) GLOBAL_UNIT_ASSIGNED_CONTEXT ( ( #5795, #7591, #3345 ) ) REPRESENTATION_CONTEXT ( 'NONE', 'WORKASPACE' ) );
#2703 = CARTESIAN_POINT ( 'NONE',  ( -7.184516996212029076E-14, 149.9999999999998295, 12.50000000000000000 ) ) ;
#2704 = ORIENTED_EDGE ( 'NONE', *, *, #2580, .F. ) ;
#2705 = LINE ( 'NONE', #856, #6234 ) ;
#2706 = DIRECTION ( 'NONE',  ( -0.000000000000000000, -0.000000000000000000, -1.000000000000000000 ) ) ;
#2707 = DIRECTION ( 'NONE',  ( -0.000000000000000000, -0.000000000000000000, -1.000000000000000000 ) ) ;
#2708 = FACE_OUTER_BOUND ( 'NONE', #5577, .T. ) ;
#2709 = ORIENTED_EDGE ( 'NONE', *, *, #5627, .F. ) ;
#2710 = PRODUCT_DEFINITION_SHAPE ( 'NONE', 'NONE',  #4720 ) ;
#2711 = PLANE ( 'NONE',  #6351 ) ;
#2712 = UNCERTAINTY_MEASURE_WITH_UNIT (LENGTH_MEASURE( 1.000000000000000082E-05 ), #7252, 'distance_accuracy_value', 'NONE');
#2713 = ORIENTED_EDGE ( 'NONE', *, *, #3081, .F. ) ;
#2714 = CYLINDRICAL_SURFACE ( 'NONE', #2194, 20.00000000000000000 ) ;
#2715 = EDGE_LOOP ( 'NONE', ( #2622, #4121, #6142, #2686 ) ) ;
#2716 = DIRECTION ( 'NONE',  ( -0.8886649088774988270, -0.4585571717133501424, 0.000000000000000000 ) ) ;
#2717 = DIRECTION ( 'NONE',  ( 0.000000000000000000, 0.000000000000000000, 1.000000000000000000 ) ) ;
#2718 = EDGE_CURVE ( 'NONE', #1234, #3264, #6598, .T. ) ;
#2719 = LINE ( 'NONE', #7456, #7654 ) ;
#2720 = CARTESIAN_POINT ( 'NONE',  ( 190.0000000000000000, 0.000000000000000000, 0.000000000000000000 ) ) ;
#2721 = EDGE_CURVE ( 'NONE', #6773, #3816, #6660, .T. ) ;
#2722 = ORIENTED_EDGE ( 'NONE', *, *, #7621, .F. ) ;
#2723 = CARTESIAN_POINT ( 'NONE',  ( -31.24999999999997158, 177.4999999999999432, 130.0000000000000000 ) ) ;
#2724 = VERTEX_POINT ( 'NONE', #5455 ) ;
#2725 = ORIENTED_EDGE ( 'NONE', *, *, #7391, .F. ) ;
#2726 = CARTESIAN_POINT ( 'NONE',  ( 10.82531754730548279, -13.74999999999999645, 7.500000000000000000 ) ) ;
#2727 = EDGE_CURVE ( 'NONE', #4433, #1919, #4686, .T. ) ;
#2728 = CARTESIAN_POINT ( 'NONE',  ( 296.6025403784439050, 75.00000000000007105, 12.50000000000000000 ) ) ;
#2729 = CARTESIAN_POINT ( 'NONE',  ( 42.50000000000000711, 177.5000000000000000, 0.000000000000000000 ) ) ;
#2730 = CYLINDRICAL_SURFACE ( 'NONE', #3650, 12.50000000000001066 ) ;
#2731 = ADVANCED_FACE ( 'NONE', ( #2897 ), #3533, .F. ) ;
#2732 = VECTOR ( 'NONE', #4855, 999.9999999999998863 ) ;
#2733 = ORIENTED_EDGE ( 'NONE', *, *, #4929, .T. ) ;
#2734 = EDGE_CURVE ( 'NONE', #7564, #6254, #3269, .T. ) ;
#2735 = CONTEXT_DEPENDENT_SHAPE_REPRESENTATION ( #6498, #7333 ) ;
#2736 = DIRECTION ( 'NONE',  ( 1.000000000000000000, 0.000000000000000000, 0.000000000000000000 ) ) ;
#2737 = DIRECTION ( 'NONE',  ( 0.000000000000000000, 0.000000000000000000, 1.000000000000000000 ) ) ;
#2738 = LINE ( 'NONE', #7551, #1971 ) ;
#2739 = CIRCLE ( 'NONE', #4775, 30.00000000000000000 ) ;
#2740 = PLANE ( 'NONE',  #5038 ) ;
#2741 = LINE ( 'NONE', #1017, #1857 ) ;
#2742 = VECTOR ( 'NONE', #4506, 1000.000000000000000 ) ;
#2743 = LINE ( 'NONE', #1415, #6256 ) ;
#2744 = ORIENTED_EDGE ( 'NONE', *, *, #855, .T. ) ;
#2745 = CARTESIAN_POINT ( 'NONE',  ( 18.76388374866283471, -1.044563157018773529E-16, 0.000000000000000000 ) ) ;
#2746 = DIRECTION ( 'NONE',  ( 2.960594732333750117E-15, -1.000000000000000000, 0.000000000000000000 ) ) ;
#2747 = LINE ( 'NONE', #4021, #3381 ) ;
#2748 = APPLICATION_CONTEXT ( 'automotive_design' ) ;
#2749 = ADVANCED_FACE ( 'NONE', ( #7222 ), #6694, .T. ) ;
#2750 = SURFACE_SIDE_STYLE ('',( #4701 ) ) ;
#2751 = ORIENTED_EDGE ( 'NONE', *, *, #3784, .T. ) ;
#2752 = CIRCLE ( 'NONE', #1461, 5.000000000000000888 ) ;
#2753 = CIRCLE ( 'NONE', #4405, 32.75000000000000000 ) ;
#2754 = ORIENTED_EDGE ( 'NONE', *, *, #7145, .T. ) ;
#2755 = VECTOR ( 'NONE', #2197, 1000.000000000000000 ) ;
#2756 = FACE_OUTER_BOUND ( 'NONE', #238, .T. ) ;
#2757 = CIRCLE ( 'NONE', #2371, 35.78244274809159720 ) ;
#2758 = ORIENTED_EDGE ( 'NONE', *, *, #3855, .T. ) ;
#2759 = FACE_OUTER_BOUND ( 'NONE', #7413, .T. ) ;
#2760 = CARTESIAN_POINT ( 'NONE',  ( 42.08354679051384295, 47.50000000000003553, 12.55124306091975583 ) ) ;
#2761 = CARTESIAN_POINT ( 'NONE',  ( 0.000000000000000000, 177.4999999999999432, 12.50000000000000000 ) ) ;
#2762 = CARTESIAN_POINT ( 'NONE',  ( 340.0000000000000000, 0.000000000000000000, 0.000000000000000000 ) ) ;
#2763 = CIRCLE ( 'NONE', #7249, 5.000000000000004441 ) ;
#2764 = ORIENTED_EDGE ( 'NONE', *, *, #3220, .T. ) ;
#2765 = DIRECTION ( 'NONE',  ( 1.000000000000000000, 0.000000000000000000, 0.000000000000000000 ) ) ;
#2766 = VERTEX_POINT ( 'NONE', #4726 ) ;
#2767 = LINE ( 'NONE', #5199, #70 ) ;
#2768 = ORIENTED_EDGE ( 'NONE', *, *, #5420, .T. ) ;
#2769 = CARTESIAN_POINT ( 'NONE',  ( 12.50000000000000000, 1.530808498934191127E-15, 45.00000000000000000 ) ) ;
#2770 = CARTESIAN_POINT ( 'NONE',  ( -31.24999999999997158, 144.7499999999999432, 130.0000000000000000 ) ) ;
#2771 = DIRECTION ( 'NONE',  ( 0.000000000000000000, 0.000000000000000000, 1.000000000000000000 ) ) ;
#2772 = MECHANICAL_DESIGN_GEOMETRIC_PRESENTATION_REPRESENTATION (  '', ( #6359 ), #720 ) ;
#2773 = ADVANCED_FACE ( 'NONE', ( #4125, #3055 ), #6577, .F. ) ;
#2774 = ORIENTED_EDGE ( 'NONE', *, *, #1980, .T. ) ;
#2775 = EDGE_CURVE ( 'NONE', #5735, #3550, #7143, .T. ) ;
#2776 = PRODUCT ( 'Bolt1', 'Bolt1', '', ( #1733 ) ) ;
#2777 = CARTESIAN_POINT ( 'NONE',  ( 12.50000000000000000, 1.530808498934191521E-15, 25.00000000000000000 ) ) ;
#2778 = LINE ( 'NONE', #848, #4332 ) ;
#2780 = CARTESIAN_POINT ( 'NONE',  ( 42.50000000000000000, 42.50000000000003553, 0.000000000000000000 ) ) ;
#2779 = PRESENTATION_LAYER_ASSIGNMENT (  '', '', ( #4056 ) ) ;
#2781 = PLANE ( 'NONE',  #5430 ) ;
#2782 = CARTESIAN_POINT ( 'NONE',  ( 46.25000000000002842, 47.50000000000003553, 130.0000000000000000 ) ) ;
#2783 = ADVANCED_FACE ( 'NONE', ( #1043 ), #2938, .T. ) ;
#2784 = CIRCLE ( 'NONE', #3425, 12.50000000000001066 ) ;
#2785 = DIRECTION ( 'NONE',  ( 4.270088556250607616E-16, 1.000000000000000000, 0.000000000000000000 ) ) ;
#2786 =( LENGTH_UNIT ( ) NAMED_UNIT ( * ) SI_UNIT ( .MILLI., .METRE. ) );
#2787 = ORIENTED_EDGE ( 'NONE', *, *, #6280, .F. ) ;
#2788 = DIRECTION ( 'NONE',  ( -0.000000000000000000, -0.000000000000000000, -1.000000000000000000 ) ) ;
#2789 = DIRECTION ( 'NONE',  ( -0.000000000000000000, 0.000000000000000000, 1.000000000000000000 ) ) ;
#2790 = FACE_BOUND ( 'NONE', #3191, .T. ) ;
#2791 = ORIENTED_EDGE ( 'NONE', *, *, #5682, .T. ) ;
#2792 = ORIENTED_EDGE ( 'NONE', *, *, #967, .F. ) ;
#2793 = EDGE_CURVE ( 'NONE', #5569, #1300, #4164, .T. ) ;
#2794 = VECTOR ( 'NONE', #1162, 1000.000000000000000 ) ;
#2795 = AXIS2_PLACEMENT_3D ( 'NONE', #4505, #381, #6316 ) ;
#2796 = DIRECTION ( 'NONE',  ( 0.000000000000000000, -0.000000000000000000, -1.000000000000000000 ) ) ;
#2797 = ORIENTED_EDGE ( 'NONE', *, *, #4772, .F. ) ;
#2798 = CARTESIAN_POINT ( 'NONE',  ( 0.000000000000000000, 0.000000000000000000, 25.00000000000000000 ) ) ;
#2799 = CARTESIAN_POINT ( 'NONE',  ( 1.320471425210250835E-15, 3.061616997868383043E-15, -25.00000000000000000 ) ) ;
#2800 = ORIENTED_EDGE ( 'NONE', *, *, #1263, .T. ) ;
#2801 = PLANE ( 'NONE',  #7025 ) ;
#2802 = DIRECTION ( 'NONE',  ( -4.789677997474686366E-16, -1.000000000000000000, 0.000000000000000000 ) ) ;
#2803 = CIRCLE ( 'NONE', #6380, 5.000000000000000000 ) ;
#2804 = AXIS2_PLACEMENT_3D ( 'NONE', #1258, #6153, #1296 ) ;
#2805 = ORIENTED_EDGE ( 'NONE', *, *, #2775, .T. ) ;
#2806 = EDGE_CURVE ( 'NONE', #3331, #308, #6022, .T. ) ;
#2807 = DIRECTION ( 'NONE',  ( 0.000000000000000000, 0.000000000000000000, 1.000000000000000000 ) ) ;
#2808 = VERTEX_POINT ( 'NONE', #755 ) ;
#2809 = AXIS2_PLACEMENT_3D ( 'NONE', #6413, #5736, #2159 ) ;
#2810 = CARTESIAN_POINT ( 'NONE',  ( 6.249999999999977796, 0.000000000000000000, 0.000000000000000000 ) ) ;
#2811 = VECTOR ( 'NONE', #1842, 1000.000000000000000 ) ;
#2812 = ORIENTED_EDGE ( 'NONE', *, *, #5620, .T. ) ;
#2813 = CARTESIAN_POINT ( 'NONE',  ( 0.000000000000000000, 0.000000000000000000, 7.500000000000000000 ) ) ;
#2814 = CARTESIAN_POINT ( 'NONE',  ( -0.000000000000000000, -5.595828947448873159, 0.000000000000000000 ) ) ;
#2815 = CARTESIAN_POINT ( 'NONE',  ( 0.000000000000000000, 0.000000000000000000, 0.000000000000000000 ) ) ;
#2816 = VECTOR ( 'NONE', #599, 1000.000000000000000 ) ;
#2817 = VECTOR ( 'NONE', #5732, 1000.000000000000000 ) ;
#2818 = ORIENTED_EDGE ( 'NONE', *, *, #2125, .T. ) ;
#2819 = DIRECTION ( 'NONE',  ( -0.000000000000000000, -0.000000000000000000, -1.000000000000000000 ) ) ;
#2820 = DIRECTION ( 'NONE',  ( 0.8886649088774989380, -0.4585571717133497538, 0.000000000000000000 ) ) ;
#2821 = DIRECTION ( 'NONE',  ( 0.000000000000000000, 0.000000000000000000, 1.000000000000000000 ) ) ;
#2822 = DIRECTION ( 'NONE',  ( 0.000000000000000000, -1.387778780781445676E-16, 1.000000000000000000 ) ) ;
#2823 = EDGE_CURVE ( 'NONE', #5267, #3802, #115, .T. ) ;
#2824 = DIRECTION ( 'NONE',  ( 0.000000000000000000, 0.000000000000000000, 1.000000000000000000 ) ) ;
#2825 = EDGE_CURVE ( 'NONE', #603, #5920, #5705, .T. ) ;
#2826 = CARTESIAN_POINT ( 'NONE',  ( 0.000000000000000000, 0.000000000000000000, 0.000000000000000000 ) ) ;
#2827 = DIRECTION ( 'NONE',  ( 1.000000000000000000, -4.789593822244094799E-16, -4.789593822244094799E-16 ) ) ;
#2828 = ORIENTED_EDGE ( 'NONE', *, *, #1346, .T. ) ;
#2829 = LINE ( 'NONE', #380, #1623 ) ;
#2830 = CARTESIAN_POINT ( 'NONE',  ( 2.775557561562891351E-14, 225.0000000000000284, 12.50000000000000000 ) ) ;
#2831 = DIRECTION ( 'NONE',  ( -1.000000000000000000, 0.000000000000000000, 0.000000000000000000 ) ) ;
#2832 = ADVANCED_FACE ( 'NONE', ( #1833 ), #3696, .T. ) ;
#2833 = DIRECTION ( 'NONE',  ( 1.000000000000000000, 0.000000000000000000, 0.000000000000000000 ) ) ;
#2834 = ORIENTED_EDGE ( 'NONE', *, *, #5816, .F. ) ;
#2835 = ADVANCED_FACE ( 'NONE', ( #3132, #6137, #4881 ), #6778, .F. ) ;
#2836 = CONICAL_SURFACE ( 'NONE', #12, 15.00000000000000000, 0.7853981633974479459 ) ;
#2837 = ORIENTED_EDGE ( 'NONE', *, *, #5185, .F. ) ;
#2838 = VERTEX_POINT ( 'NONE', #6251 ) ;
#2839 =( NAMED_UNIT ( * ) SI_UNIT ( $, .STERADIAN. ) SOLID_ANGLE_UNIT ( ) );
#2840 = ORIENTED_EDGE ( 'NONE', *, *, #4499, .T. ) ;
#2841 = EDGE_CURVE ( 'NONE', #342, #3644, #1993, .T. ) ;
#2842 = CARTESIAN_POINT ( 'NONE',  ( 0.7190441502950353225, 62.70544120911855401, 12.50000000000000000 ) ) ;
#2843 = VERTEX_POINT ( 'NONE', #7421 ) ;
#2844 = CIRCLE ( 'NONE', #1529, 20.00000000000000000 ) ;
#2845 = EDGE_LOOP ( 'NONE', ( #4840, #487, #2525, #4909 ) ) ;
#2846 = FACE_OUTER_BOUND ( 'NONE', #5534, .T. ) ;
#2847 = DIRECTION ( 'NONE',  ( -1.000000000000000000, -0.000000000000000000, -0.000000000000000000 ) ) ;
#2848 = PRODUCT ( 'Bushing', 'Bushing', '', ( #6789 ) ) ;
#2849 = ORIENTED_EDGE ( 'NONE', *, *, #3726, .T. ) ;
#2850 = CARTESIAN_POINT ( 'NONE',  ( 0.000000000000000000, 2.296212748401299411E-15, 18.75000000000009948 ) ) ;
#2851 = ORIENTED_EDGE ( 'NONE', *, *, #374, .T. ) ;
#2852 = DIRECTION ( 'NONE',  ( 1.000000000000000000, 0.000000000000000000, 0.000000000000000000 ) ) ;
#2853 = VERTEX_POINT ( 'NONE', #1282 ) ;
#2854 = CYLINDRICAL_SURFACE ( 'NONE', #2286, 65.50000000000000000 ) ;
#2855 = FACE_OUTER_BOUND ( 'NONE', #4520, .T. ) ;
#2856 = DIRECTION ( 'NONE',  ( -0.5000000000000002220, -0.8660254037844384856, 0.000000000000000000 ) ) ;
#2857 = DIRECTION ( 'NONE',  ( -1.000000000000000000, -0.000000000000000000, 0.000000000000000000 ) ) ;
#2858 = EDGE_CURVE ( 'NONE', #5119, #6483, #3806, .T. ) ;
#2859 = EDGE_LOOP ( 'NONE', ( #7283, #3113 ) ) ;
#2860 = VERTEX_POINT ( 'NONE', #154 ) ;
#2861 = DIRECTION ( 'NONE',  ( -0.000000000000000000, -0.000000000000000000, -1.000000000000000000 ) ) ;
#2862 = CARTESIAN_POINT ( 'NONE',  ( 0.000000000000000000, 0.000000000000000000, 25.00000000000000000 ) ) ;
#2863 = PLANE ( 'NONE',  #2210 ) ;
#2864 = CARTESIAN_POINT ( 'NONE',  ( 291.6025403784439050, 90.00000000000001421, 0.000000000000000000 ) ) ;
#2865 = CARTESIAN_POINT ( 'NONE',  ( 379.0974461856235393, 16.13667248250984798, 11.81655595281366899 ) ) ;
#2866 = DIRECTION ( 'NONE',  ( -0.000000000000000000, 0.000000000000000000, 1.000000000000000000 ) ) ;
#2867 = DIRECTION ( 'NONE',  ( 0.9753188030613186843, -4.670859075146478753E-16, 0.2208013414701927302 ) ) ;
#2868 = EDGE_LOOP ( 'NONE', ( #2031, #7809 ) ) ;
#2869 = DIRECTION ( 'NONE',  ( -0.5000000000000004441, -0.8660254037844383745, 0.000000000000000000 ) ) ;
#2870 = CARTESIAN_POINT ( 'NONE',  ( 340.0000000000000000, 25.00000000000000000, 0.000000000000000000 ) ) ;
#2871 = FACE_BOUND ( 'NONE', #5231, .T. ) ;
#2872 = ORIENTED_EDGE ( 'NONE', *, *, #666, .T. ) ;
#2873 = PRODUCT_DEFINITION_CONTEXT ( 'detailed design', #244, 'design' ) ;
#2874 = CIRCLE ( 'NONE', #3891, 12.50000000000000355 ) ;
#2875 = ORIENTED_EDGE ( 'NONE', *, *, #2825, .F. ) ;
#2876 = VERTEX_POINT ( 'NONE', #2599 ) ;
#2877 = EDGE_CURVE ( 'NONE', #4540, #3234, #5614, .T. ) ;
#2878 = ORIENTED_EDGE ( 'NONE', *, *, #7730, .F. ) ;
#2879 = CARTESIAN_POINT ( 'NONE',  ( 412.5000000000000568, 80.00000000000001421, 0.000000000000000000 ) ) ;
#2881 = CYLINDRICAL_SURFACE ( 'NONE', #3130, 5.000000000000004441 ) ;
#2880 = CIRCLE ( 'NONE', #7748, 12.50000000000000355 ) ;
#2882 = ADVANCED_FACE ( 'NONE', ( #2522 ), #1874, .F. ) ;
#2883 = AXIS2_PLACEMENT_3D ( 'NONE', #3334, #7543, #6977 ) ;
#2884 = ORIENTED_EDGE ( 'NONE', *, *, #3057, .F. ) ;
#2885 = DIRECTION ( 'NONE',  ( -0.000000000000000000, -0.000000000000000000, -1.000000000000000000 ) ) ;
#2886 = CARTESIAN_POINT ( 'NONE',  ( -25.00000000000000000, 25.00000000000000000, 0.000000000000000000 ) ) ;
#2887 = AXIS2_PLACEMENT_3D ( 'NONE', #7457, #5494, #1917 ) ;
#2888 = EDGE_CURVE ( 'NONE', #4514, #4723, #1950, .T. ) ;
#2889 = ORIENTED_EDGE ( 'NONE', *, *, #2901, .T. ) ;
#2890 = CIRCLE ( 'NONE', #4664, 25.00000000000000000 ) ;
#2891 = LINE ( 'NONE', #3006, #3958 ) ;
#2892 = ORIENTED_EDGE ( 'NONE', *, *, #6722, .F. ) ;
#2893 = DIRECTION ( 'NONE',  ( -1.000000000000000000, -0.000000000000000000, -0.000000000000000000 ) ) ;
#2894 = ORIENTED_EDGE ( 'NONE', *, *, #2342, .F. ) ;
#2895 = CARTESIAN_POINT ( 'NONE',  ( 200.0000000000000000, 0.000000000000000000, 12.50000000000000000 ) ) ;
#2896 = AXIS2_PLACEMENT_3D ( 'NONE', #1273, #6725, #60 ) ;
#2897 = FACE_OUTER_BOUND ( 'NONE', #7287, .T. ) ;
#2898 = ORIENTED_EDGE ( 'NONE', *, *, #5147, .F. ) ;
#2899 = AXIS2_PLACEMENT_3D ( 'NONE', #5284, #1680, #956 ) ;
#2900 = VERTEX_POINT ( 'NONE', #1394 ) ;
#2901 = EDGE_CURVE ( 'NONE', #345, #3167, #716, .T. ) ;
#2902 = DIRECTION ( 'NONE',  ( -0.000000000000000000, -0.000000000000000000, -1.000000000000000000 ) ) ;
#2903 = DIRECTION ( 'NONE',  ( 1.000000000000000000, 0.000000000000000000, 0.000000000000000000 ) ) ;
#2904 = DIRECTION ( 'NONE',  ( -0.000000000000000000, 0.000000000000000000, -1.000000000000000000 ) ) ;
#2905 = LINE ( 'NONE', #615, #6706 ) ;
#2906 = AXIS2_PLACEMENT_3D ( 'NONE', #2810, #6452, #5329 ) ;
#2907 = CARTESIAN_POINT ( 'NONE',  ( 380.5932282495298864, 16.58082631454064781, 11.18611842067925011 ) ) ;
#2908 = SHAPE_REPRESENTATION ( 'Bushing', ( #5785 ), #4233 ) ;
#2909 = DIRECTION ( 'NONE',  ( -0.000000000000000000, 0.000000000000000000, -1.000000000000000000 ) ) ;
#2910 = PRESENTATION_LAYER_ASSIGNMENT (  '', '', ( #6359 ) ) ;
#2911 = APPLICATION_PROTOCOL_DEFINITION ( 'draft international standard', 'automotive_design', 1998, #7820 ) ;
#2912 = ORIENTED_EDGE ( 'NONE', *, *, #7394, .T. ) ;
#2913 = CARTESIAN_POINT ( 'NONE',  ( -37.49999999999992184, 112.5000000000000142, 195.4980915752512658 ) ) ;
#2914 = DIRECTION ( 'NONE',  ( 1.000000000000000000, 0.000000000000000000, 0.000000000000000000 ) ) ;
#2915 = PLANE ( 'NONE',  #1213 ) ;
#2916 = FACE_BOUND ( 'NONE', #647, .T. ) ;
#2917 = ORIENTED_EDGE ( 'NONE', *, *, #6151, .T. ) ;
#2918 = COLOUR_RGB ( '',0.7921568627450980005, 0.8196078431372548767, 0.9333333333333333481 ) ;
#2919 = EDGE_CURVE ( 'NONE', #2226, #4382, #55, .T. ) ;
#2920 = ORIENTED_EDGE ( 'NONE', *, *, #1349, .T. ) ;
#2921 = ORIENTED_EDGE ( 'NONE', *, *, #4528, .T. ) ;
#2922 = CIRCLE ( 'NONE', #7144, 12.50000000000000000 ) ;
#2923 = CARTESIAN_POINT ( 'NONE',  ( 296.6025403784437913, 142.5000000000000000, 17.49999999999998934 ) ) ;
#2924 = ORIENTED_EDGE ( 'NONE', *, *, #5154, .F. ) ;
#2925 = DIRECTION ( 'NONE',  ( 1.000000000000000000, 0.000000000000000000, 0.000000000000000000 ) ) ;
#2926 = EDGE_CURVE ( 'NONE', #6684, #3810, #5036, .T. ) ;
#2927 = AXIS2_PLACEMENT_3D ( 'NONE', #4400, #3333, #2567 ) ;
#2928 = EDGE_CURVE ( 'NONE', #221, #1390, #2446, .T. ) ;
#2929 = ORIENTED_EDGE ( 'NONE', *, *, #5293, .F. ) ;
#2930 = CARTESIAN_POINT ( 'NONE',  ( 296.6025403784437913, 82.50000000000004263, 17.49999999999998934 ) ) ;
#2931 = ORIENTED_EDGE ( 'NONE', *, *, #5766, .T. ) ;
#2932 = CARTESIAN_POINT ( 'NONE',  ( 375.0000000000000000, -15.61249499599599488, 12.50000000000000711 ) ) ;
#2933 = ORIENTED_EDGE ( 'NONE', *, *, #1960, .T. ) ;
#2934 = CIRCLE ( 'NONE', #1131, 20.00000000000000000 ) ;
#2935 = DIRECTION ( 'NONE',  ( -0.000000000000000000, 0.000000000000000000, 1.000000000000000000 ) ) ;
#2936 = AXIS2_PLACEMENT_3D ( 'NONE', #3231, #664, #5553 ) ;
#2937 = EDGE_CURVE ( 'NONE', #4729, #6728, #4319, .T. ) ;
#2938 = PLANE ( 'NONE',  #6215 ) ;
#2939 = ADVANCED_FACE ( 'NONE', ( #677 ), #4793, .T. ) ;
#2940 = VERTEX_POINT ( 'NONE', #3770 ) ;
#2941 = VECTOR ( 'NONE', #6517, 1000.000000000000227 ) ;
#2942 = CIRCLE ( 'NONE', #1648, 12.50000000000001066 ) ;
#2943 = EDGE_LOOP ( 'NONE', ( #4086, #1430, #5952, #2694 ) ) ;
#2944 = CARTESIAN_POINT ( 'NONE',  ( -6.495190528383287365, 11.25000000000000000, 0.000000000000000000 ) ) ;
#2945 = ADVANCED_FACE ( 'NONE', ( #3994 ), #5078, .T. ) ;
#2946 = DIRECTION ( 'NONE',  ( 0.000000000000000000, 0.000000000000000000, 1.000000000000000000 ) ) ;
#2947 = CARTESIAN_POINT ( 'NONE',  ( 353.4483633286965301, 75.00000000000004263, 138.3903618369216417 ) ) ;
#2948 = CARTESIAN_POINT ( 'NONE',  ( -25.00000000000000000, -25.00000000000000000, 50.00000000000000000 ) ) ;
#2949 = AXIS2_PLACEMENT_3D ( 'NONE', #5852, #309, #2765 ) ;
#2950 = AXIS2_PLACEMENT_3D ( 'NONE', #6224, #1808, #572 ) ;
#2951 = CARTESIAN_POINT ( 'NONE',  ( 385.7933296785779476, 18.97948036624223533, -6.318259067610828339 ) ) ;
#2952 = CARTESIAN_POINT ( 'NONE',  ( 200.0000000000000000, 0.000000000000000000, 12.50000000000000000 ) ) ;
#2953 = DIRECTION ( 'NONE',  ( 1.000000000000000000, 0.000000000000000000, 0.000000000000000000 ) ) ;
#2954 = LINE ( 'NONE', #2311, #2006 ) ;
#2955 = CARTESIAN_POINT ( 'NONE',  ( -49.28095584970496645, -62.29455879088143888, 12.50000000000000000 ) ) ;
#2956 = FACE_BOUND ( 'NONE', #5681, .T. ) ;
#2957 = DIRECTION ( 'NONE',  ( 0.5000000000000004441, 0.8660254037844383745, 0.000000000000000000 ) ) ;
#2958 = ORIENTED_EDGE ( 'NONE', *, *, #147, .T. ) ;
#2959 = EDGE_CURVE ( 'NONE', #1785, #1677, #6368, .T. ) ;
#2960 = PRODUCT_DEFINITION_CONTEXT ( 'detailed design', #6798, 'design' ) ;
#2961 = ORIENTED_EDGE ( 'NONE', *, *, #3513, .T. ) ;
#2962 =( LENGTH_UNIT ( ) NAMED_UNIT ( * ) SI_UNIT ( .MILLI., .METRE. ) );
#2963 = EDGE_LOOP ( 'NONE', ( #3159, #7017, #95, #5411, #1744, #7497, #2689 ) ) ;
#2964 = SURFACE_STYLE_USAGE ( .BOTH. , #1860 ) ;
#2965 = CARTESIAN_POINT ( 'NONE',  ( -6.495190528383282036, -11.24999999999999645, 7.500000000000000000 ) ) ;
#2966 = VERTEX_POINT ( 'NONE', #7052 ) ;
#2967 = CARTESIAN_POINT ( 'NONE',  ( -12.49999999999996803, 225.0000000000000284, 12.50000000000000000 ) ) ;
#2968 = ORIENTED_EDGE ( 'NONE', *, *, #6346, .T. ) ;
#2969 = DIRECTION ( 'NONE',  ( -0.000000000000000000, 0.000000000000000000, 1.000000000000000000 ) ) ;
#2970 = EDGE_LOOP ( 'NONE', ( #3840, #6213, #73, #7376 ) ) ;
#2971 = EDGE_CURVE ( 'NONE', #1320, #3444, #4538, .T. ) ;
#2972 = CARTESIAN_POINT ( 'NONE',  ( 372.8893025888656894, -15.74939801616919866, -12.32751675873151598 ) ) ;
#2973 = VERTEX_POINT ( 'NONE', #1514 ) ;
#2974 = LINE ( 'NONE', #6776, #7020 ) ;
#2975 = CARTESIAN_POINT ( 'NONE',  ( 162.4999999999999432, 187.4999999999999716, 12.50000000000000000 ) ) ;
#2976 = AXIS2_PLACEMENT_3D ( 'NONE', #2990, #463, #7758 ) ;
#2977 = VERTEX_POINT ( 'NONE', #7531 ) ;
#2978 = ORIENTED_EDGE ( 'NONE', *, *, #5093, .T. ) ;
#2979 = EDGE_CURVE ( 'NONE', #2146, #6485, #4598, .T. ) ;
#2980 = CARTESIAN_POINT ( 'NONE',  ( 0.000000000000000000, 0.000000000000000000, 35.78244274809159720 ) ) ;
#2981 = DIRECTION ( 'NONE',  ( -0.000000000000000000, -0.000000000000000000, -1.000000000000000000 ) ) ;
#2982 = CARTESIAN_POINT ( 'NONE',  ( 0.000000000000000000, 0.000000000000000000, 97.50000000000000000 ) ) ;
#2983 = CARTESIAN_POINT ( 'NONE',  ( 286.6025403784437913, 0.000000000000000000, 12.50000000000000000 ) ) ;
#2984 = EDGE_CURVE ( 'NONE', #6898, #6728, #910, .T. ) ;
#2985 = DIRECTION ( 'NONE',  ( -4.237492460401359023E-16, -1.000000000000000000, 0.000000000000000000 ) ) ;
#2986 = DIRECTION ( 'NONE',  ( -0.000000000000000000, -0.000000000000000000, -1.000000000000000000 ) ) ;
#2987 = EDGE_CURVE ( 'NONE', #2, #1820, #7608, .T. ) ;
#2988 = EDGE_CURVE ( 'NONE', #2325, #5081, #2113, .T. ) ;
#2989 = FACE_OUTER_BOUND ( 'NONE', #3043, .T. ) ;
#2990 = CARTESIAN_POINT ( 'NONE',  ( 364.5325195641692062, 209.6990734970208337, 283.9062424146593457 ) ) ;
#2991 = DIRECTION ( 'NONE',  ( 1.000000000000000000, 0.000000000000000000, 0.000000000000000000 ) ) ;
#2992 = LINE ( 'NONE', #4658, #7157 ) ;
#2993 = DIRECTION ( 'NONE',  ( 0.000000000000000000, -1.387778780781445676E-16, 1.000000000000000000 ) ) ;
#2994 = CARTESIAN_POINT ( 'NONE',  ( 0.000000000000000000, 47.50000000000009237, 12.50000000000000000 ) ) ;
#2995 = EDGE_LOOP ( 'NONE', ( #3317, #5151, #7053, #3614 ) ) ;
#2996 = EDGE_LOOP ( 'NONE', ( #5743, #7692, #228, #6782, #5229, #7208, #3505, #7006 ) ) ;
#2997 = AXIS2_PLACEMENT_3D ( 'NONE', #7430, #1171, #1925 ) ;
#2998 = VERTEX_POINT ( 'NONE', #5194 ) ;
#2999 = EDGE_CURVE ( 'NONE', #7266, #2808, #1847, .T. ) ;
#3000 = FACE_BOUND ( 'NONE', #3120, .T. ) ;
#3001 = CYLINDRICAL_SURFACE ( 'NONE', #2487, 12.50000000000001066 ) ;
#3002 = EDGE_LOOP ( 'NONE', ( #6120, #5755, #1280, #6389 ) ) ;
#3003 = AXIS2_PLACEMENT_3D ( 'NONE', #2994, #4863, #7909 ) ;
#3004 = DIRECTION ( 'NONE',  ( -0.000000000000000000, -0.000000000000000000, -1.000000000000000000 ) ) ;
#3005 = VERTEX_POINT ( 'NONE', #7088 ) ;
#3006 = CARTESIAN_POINT ( 'NONE',  ( 47.50000000000000711, 0.000000000000000000, 0.000000000000000000 ) ) ;
#3007 = ORIENTED_EDGE ( 'NONE', *, *, #3636, .F. ) ;
#3008 = VECTOR ( 'NONE', #6433, 1000.000000000000000 ) ;
#3009 = CARTESIAN_POINT ( 'NONE',  ( 369.3727881274253946, -16.58005916595991280, -11.19168395254304471 ) ) ;
#3010 = ORIENTED_EDGE ( 'NONE', *, *, #6531, .T. ) ;
#3011 = CARTESIAN_POINT ( 'NONE',  ( 25.71904415029483459, 19.40417101989674009, 0.000000000000000000 ) ) ;
#3012 = APPLICATION_CONTEXT ( 'automotive_design' ) ;
#3013 = DIRECTION ( 'NONE',  ( -0.000000000000000000, -0.000000000000000000, -1.000000000000000000 ) ) ;
#3014 = AXIS2_PLACEMENT_3D ( 'NONE', #7263, #2406, #2329 ) ;
#3015 = CIRCLE ( 'NONE', #5048, 31.25000000000000000 ) ;
#3016 = VECTOR ( 'NONE', #326, 1000.000000000000000 ) ;
#3017 = ORIENTED_EDGE ( 'NONE', *, *, #5069, .F. ) ;
#3018 = VERTEX_POINT ( 'NONE', #2642 ) ;
#3019 = AXIS2_PLACEMENT_3D ( 'NONE', #3242, #5692, #189 ) ;
#3020 = CARTESIAN_POINT ( 'NONE',  ( 385.8076615439897523, -18.98451973267744464, 6.332666029034883515 ) ) ;
#3021 = AXIS2_PLACEMENT_3D ( 'NONE', #6755, #1739, #1819 ) ;
#3022 = CARTESIAN_POINT ( 'NONE',  ( 0.000000000000000000, 0.000000000000000000, 2.500000000000085265 ) ) ;
#3023 = CARTESIAN_POINT ( 'NONE',  ( -49.28095584970496645, -62.29455879088143888, 0.000000000000000000 ) ) ;
#3024 = LINE ( 'NONE', #7312, #2732 ) ;
#3025 = DIRECTION ( 'NONE',  ( -1.000000000000000000, -1.261617073437677999E-16, 0.000000000000000000 ) ) ;
#3026 = CARTESIAN_POINT ( 'NONE',  ( -12.50000000000000000, 0.000000000000000000, 90.00000000000000000 ) ) ;
#3027 = EDGE_CURVE ( 'NONE', #2041, #5081, #4923, .T. ) ;
#3028 = VECTOR ( 'NONE', #892, 1000.000000000000227 ) ;
#3029 = ADVANCED_FACE ( 'NONE', ( #832 ), #3401, .T. ) ;
#3030 = CARTESIAN_POINT ( 'NONE',  ( 0.000000000000000000, 0.000000000000000000, 82.49999999999998579 ) ) ;
#3031 = ITEM_DEFINED_TRANSFORMATION ( 'NONE', 'NONE', #6047,  #5785 ) ;
#3032 = CARTESIAN_POINT ( 'NONE',  ( 335.4891275541129971, 142.5000000000000000, 174.3961449365926626 ) ) ;
#3034 = FACE_OUTER_BOUND ( 'NONE', #3592, .T. ) ;
#3033 = AXIS2_PLACEMENT_3D ( 'NONE', #5371, #2852, #2203 ) ;
#3035 = DIRECTION ( 'NONE',  ( 0.000000000000000000, 0.000000000000000000, 1.000000000000000000 ) ) ;
#3036 = EDGE_LOOP ( 'NONE', ( #3767, #1703, #6937, #5970 ) ) ;
#3037 = AXIS2_PLACEMENT_3D ( 'NONE', #4032, #6486, #391 ) ;
#3038 = SHAPE_REPRESENTATION_RELATIONSHIP ( 'NONE' , 'NONE' ,  #1772, #4490 ) ;
#3039 = ORIENTED_EDGE ( 'NONE', *, *, #7090, .F. ) ;
#3040 = DIRECTION ( 'NONE',  ( 1.000000000000000000, 0.000000000000000000, 0.000000000000000000 ) ) ;
#3041 = CARTESIAN_POINT ( 'NONE',  ( 12.50000000000000355, 1.530808498934191521E-15, 12.50000000000000000 ) ) ;
#3042 = LINE ( 'NONE', #2251, #1848 ) ;
#3043 = EDGE_LOOP ( 'NONE', ( #2442, #1026, #2828, #3398 ) ) ;
#3044 = AXIS2_PLACEMENT_3D ( 'NONE', #2576, #5052, #768 ) ;
#3045 = CYLINDRICAL_SURFACE ( 'NONE', #5181, 37.50000000000000000 ) ;
#3046 = ADVANCED_FACE ( 'NONE', ( #5849, #4557 ), #7012, .T. ) ;
#3047 = PRODUCT_DEFINITION_SHAPE ( 'NONE', 'NONE',  #7928 ) ;
#3048 = ORIENTED_EDGE ( 'NONE', *, *, #6253, .F. ) ;
#3049 = VECTOR ( 'NONE', #7428, 1000.000000000000227 ) ;
#3050 = FACE_OUTER_BOUND ( 'NONE', #1239, .T. ) ;
#3051 = VERTEX_POINT ( 'NONE', #7691 ) ;
#3052 = CARTESIAN_POINT ( 'NONE',  ( 0.000000000000000000, 0.000000000000000000, 0.000000000000000000 ) ) ;
#3053 = VERTEX_POINT ( 'NONE', #3920 ) ;
#3054 = CARTESIAN_POINT ( 'NONE',  ( 190.0000000000000000, 1.836970198721029589E-15, -15.00000000000000000 ) ) ;
#3055 = FACE_BOUND ( 'NONE', #3679, .T. ) ;
#3056 = AXIS2_PLACEMENT_3D ( 'NONE', #2119, #6940, #4523 ) ;
#3057 = EDGE_CURVE ( 'NONE', #3356, #2392, #4633, .T. ) ;
#3058 = ORIENTED_EDGE ( 'NONE', *, *, #2888, .T. ) ;
#3059 = ORIENTED_EDGE ( 'NONE', *, *, #6061, .F. ) ;
#3060 = VECTOR ( 'NONE', #2294, 1000.000000000000000 ) ;
#3061 = VECTOR ( 'NONE', #336, 1000.000000000000000 ) ;
#3062 = ORIENTED_EDGE ( 'NONE', *, *, #5526, .F. ) ;
#3063 = CARTESIAN_POINT ( 'NONE',  ( 138.5360707071662887, -22.21662272193747256, 25.00000000000000000 ) ) ;
#3064 = CARTESIAN_POINT ( 'NONE',  ( 379.4812749451934337, -16.23897639391231706, -11.67616422689687639 ) ) ;
#3065 = DIRECTION ( 'NONE',  ( 0.000000000000000000, 0.000000000000000000, 1.000000000000000000 ) ) ;
#3066 = DIRECTION ( 'NONE',  ( -1.000000000000000000, 0.000000000000000000, 0.000000000000000000 ) ) ;
#3067 = DIRECTION ( 'NONE',  ( -0.000000000000000000, -0.000000000000000000, -1.000000000000000000 ) ) ;
#3068 = CARTESIAN_POINT ( 'NONE',  ( 386.3591492015264635, 19.30709367143974831, -5.233317247790644444 ) ) ;
#3069 = AXIS2_PLACEMENT_3D ( 'NONE', #4501, #1453, #5756 ) ;
#3070 = CONICAL_SURFACE ( 'NONE', #6136, 12.50000000000000000, 0.7853981633974521648 ) ;
#3071 = CARTESIAN_POINT ( 'NONE',  ( 400.0000000000000568, 25.00000000000000000, 0.000000000000000000 ) ) ;
#3072 = ITEM_DEFINED_TRANSFORMATION ( 'NONE', 'NONE', #782,  #5785 ) ;
#3073 = AXIS2_PLACEMENT_3D ( 'NONE', #7094, #5894, #4040 ) ;
#3074 = PRODUCT_RELATED_PRODUCT_CATEGORY ( 'part', '', ( #3858 ) ) ;
#3075 = DIRECTION ( 'NONE',  ( -1.000000000000000000, -0.000000000000000000, -0.000000000000000000 ) ) ;
#3076 = AXIS2_PLACEMENT_3D ( 'NONE', #2530, #4889, #5585 ) ;
#3077 = CARTESIAN_POINT ( 'NONE',  ( -6.495190528383282036, -11.24999999999999645, 7.500000000000000000 ) ) ;
#3078 = DIRECTION ( 'NONE',  ( 0.000000000000000000, 0.000000000000000000, 1.000000000000000000 ) ) ;
#3079 = ADVANCED_FACE ( 'NONE', ( #7570 ), #2072, .F. ) ;
#3080 = ORIENTED_EDGE ( 'NONE', *, *, #4999, .F. ) ;
#3081 = EDGE_CURVE ( 'NONE', #6638, #3115, #871, .T. ) ;
#3082 = ORIENTED_EDGE ( 'NONE', *, *, #4883, .F. ) ;
#3083 = EDGE_CURVE ( 'NONE', #3773, #4917, #6410, .T. ) ;
#3084 =( LENGTH_UNIT ( ) NAMED_UNIT ( * ) SI_UNIT ( .MILLI., .METRE. ) );
#3085 = CARTESIAN_POINT ( 'NONE',  ( 0.000000000000000000, 0.000000000000000000, 0.000000000000000000 ) ) ;
#3086 = DIRECTION ( 'NONE',  ( -1.000000000000000000, 0.000000000000000000, 0.000000000000000000 ) ) ;
#3087 = ORIENTED_EDGE ( 'NONE', *, *, #6722, .T. ) ;
#3088 = CARTESIAN_POINT ( 'NONE',  ( 2.775557561562891351E-14, 225.0000000000000284, 12.50000000000000000 ) ) ;
#3089 = ORIENTED_EDGE ( 'NONE', *, *, #470, .T. ) ;
#3090 = EDGE_CURVE ( 'NONE', #2269, #5006, #5808, .T. ) ;
#3091 = CARTESIAN_POINT ( 'NONE',  ( 372.0849291719837311, 15.87720460852527715, 12.16246356757440950 ) ) ;
#3092 = ORIENTED_EDGE ( 'NONE', *, *, #1589, .T. ) ;
#3093 = CARTESIAN_POINT ( 'NONE',  ( 363.3331590693758812, -19.48969576164946105, 4.506197270647787967 ) ) ;
#3094 = VERTEX_POINT ( 'NONE', #3560 ) ;
#3095 = DIRECTION ( 'NONE',  ( -0.000000000000000000, -0.000000000000000000, -1.000000000000000000 ) ) ;
#3096 = DIRECTION ( 'NONE',  ( 4.237492460401360996E-16, 1.000000000000000000, -1.694996984160544398E-15 ) ) ;
#3097 =( GEOMETRIC_REPRESENTATION_CONTEXT ( 3 ) GLOBAL_UNCERTAINTY_ASSIGNED_CONTEXT ( ( #3838 ) ) GLOBAL_UNIT_ASSIGNED_CONTEXT ( ( #2584, #4375, #6834 ) ) REPRESENTATION_CONTEXT ( 'NONE', 'WORKASPACE' ) );
#3098 = ORIENTED_EDGE ( 'NONE', *, *, #2806, .T. ) ;
#3099 = EDGE_LOOP ( 'NONE', ( #157, #1074, #1585, #5931 ) ) ;
#3100 = VERTEX_POINT ( 'NONE', #1633 ) ;
#3101 = CARTESIAN_POINT ( 'NONE',  ( 383.2489613821426246, -17.65558712887547443, 9.400222409301415283 ) ) ;
#3102 = EDGE_CURVE ( 'NONE', #334, #5922, #1070, .T. ) ;
#3103 = CARTESIAN_POINT ( 'NONE',  ( 286.6025403784439050, 0.000000000000000000, 12.50000000000000000 ) ) ;
#3104 = DIRECTION ( 'NONE',  ( -1.000000000000000000, 0.000000000000000000, 0.000000000000000000 ) ) ;
#3105 = CARTESIAN_POINT ( 'NONE',  ( -8.959197987552832032, 23.33951095074251114, 0.000000000000000000 ) ) ;
#3106 = PRODUCT_DEFINITION_FORMATION_WITH_SPECIFIED_SOURCE ( 'ANY', '', #3417, .NOT_KNOWN. ) ;
#3107 = DIRECTION ( 'NONE',  ( 0.000000000000000000, 1.481552359947913884E-16, -1.000000000000000000 ) ) ;
#3108 = DIRECTION ( 'NONE',  ( 0.000000000000000000, -1.694996984160544398E-15, 1.000000000000000000 ) ) ;
#3109 = LINE ( 'NONE', #5545, #2523 ) ;
#3110 = DIRECTION ( 'NONE',  ( 0.000000000000000000, 0.000000000000000000, -1.000000000000000000 ) ) ;
#3111 = CARTESIAN_POINT ( 'NONE',  ( -16.96112411586215529, 80.38061160285559481, 0.000000000000000000 ) ) ;
#3112 = CARTESIAN_POINT ( 'NONE',  ( 9.381941874331406694, 16.25000000000000000, 7.500000000000000000 ) ) ;
#3113 = ORIENTED_EDGE ( 'NONE', *, *, #1644, .T. ) ;
#3114 =( REPRESENTATION_RELATIONSHIP ('NONE','NONE', #6292, #4527 ) REPRESENTATION_RELATIONSHIP_WITH_TRANSFORMATION ( #1292 )SHAPE_REPRESENTATION_RELATIONSHIP( ) );
#3115 = VERTEX_POINT ( 'NONE', #2398 ) ;
#3116 = DIRECTION ( 'NONE',  ( 0.000000000000000000, -1.000000000000000000, 0.000000000000000000 ) ) ;
#3117 = DIRECTION ( 'NONE',  ( 1.000000000000000000, 0.000000000000000000, -0.000000000000000000 ) ) ;
#3118 = CARTESIAN_POINT ( 'NONE',  ( -37.49999999999992184, 111.9999999999999289, 130.0000000000000000 ) ) ;
#3119 = CARTESIAN_POINT ( 'NONE',  ( 42.50000000000000000, 42.50000000000003553, 12.50000000000000000 ) ) ;
#3120 = EDGE_LOOP ( 'NONE', ( #7177, #5313 ) ) ;
#3121 = DIRECTION ( 'NONE',  ( -0.000000000000000000, -0.000000000000000000, -1.000000000000000000 ) ) ;
#3122 = AXIS2_PLACEMENT_3D ( 'NONE', #6065, #6188, #573 ) ;
#3123 = EDGE_CURVE ( 'NONE', #3802, #1919, #3782, .T. ) ;
#3124 = VERTEX_POINT ( 'NONE', #557 ) ;
#3125 = EDGE_CURVE ( 'NONE', #6534, #2331, #7133, .T. ) ;
#3126 = FACE_OUTER_BOUND ( 'NONE', #7078, .T. ) ;
#3127 = ORIENTED_EDGE ( 'NONE', *, *, #2937, .F. ) ;
#3128 = CARTESIAN_POINT ( 'NONE',  ( 366.7494411481458769, -17.65634310857833356, -9.398786704980601314 ) ) ;
#3129 = ORIENTED_EDGE ( 'NONE', *, *, #2718, .F. ) ;
#3130 = AXIS2_PLACEMENT_3D ( 'NONE', #6681, #6533, #4150 ) ;
#3131 = LINE ( 'NONE', #1832, #3561 ) ;
#3132 = FACE_OUTER_BOUND ( 'NONE', #5957, .T. ) ;
#3133 = VERTEX_POINT ( 'NONE', #1753 ) ;
#3134 = VECTOR ( 'NONE', #5762, 1000.000000000000000 ) ;
#3135 = EDGE_LOOP ( 'NONE', ( #7851, #7847, #2489, #3174 ) ) ;
#3136 = ORIENTED_EDGE ( 'NONE', *, *, #5380, .T. ) ;
#3137 = CARTESIAN_POINT ( 'NONE',  ( 377.9150708280164395, -15.87720460852527715, 12.16246356757440950 ) ) ;
#3138 = CARTESIAN_POINT ( 'NONE',  ( 384.3676243783012296, -18.20590005533475875, -8.286065263872075093 ) ) ;
#3139 = CARTESIAN_POINT ( 'NONE',  ( 25.00000000000000000, -25.00000000000000000, 50.00000000000000000 ) ) ;
#3140 = DIRECTION ( 'NONE',  ( -0.9335804380297002547, -0.3583679195021130526, -0.000000000000000000 ) ) ;
#3141 = VECTOR ( 'NONE', #1343, 1000.000000000000000 ) ;
#3142 = DIRECTION ( 'NONE',  ( -1.000000000000000000, -4.789677997474691297E-16, 0.000000000000000000 ) ) ;
#3143 = ADVANCED_FACE ( 'NONE', ( #5928 ), #5830, .T. ) ;
#3144 = VECTOR ( 'NONE', #3013, 1000.000000000000000 ) ;
#3145 = CIRCLE ( 'NONE', #5706, 12.50000000000001776 ) ;
#3146 = AXIS2_PLACEMENT_3D ( 'NONE', #4768, #5865, #369 ) ;
#3147 = APPLICATION_PROTOCOL_DEFINITION ( 'draft international standard', 'automotive_design', 1998, #3218 ) ;
#3148 = DIRECTION ( 'NONE',  ( 1.000000000000000000, 0.000000000000000000, 0.000000000000000000 ) ) ;
#3149 = CYLINDRICAL_SURFACE ( 'NONE', #4204, 12.50000000000001066 ) ;
#3150 = LINE ( 'NONE', #5636, #7612 ) ;
#3151 = FACE_OUTER_BOUND ( 'NONE', #4965, .T. ) ;
#3152 = ORIENTED_EDGE ( 'NONE', *, *, #5419, .F. ) ;
#3153 = AXIS2_PLACEMENT_3D ( 'NONE', #1521, #3965, #1638 ) ;
#3154 = ORIENTED_EDGE ( 'NONE', *, *, #6118, .F. ) ;
#3155 = CARTESIAN_POINT ( 'NONE',  ( 340.0000000000000000, -12.50000000000000355, 0.000000000000000000 ) ) ;
#3156 = FACE_OUTER_BOUND ( 'NONE', #4656, .T. ) ;
#3157 = DIRECTION ( 'NONE',  ( 0.000000000000000000, 0.000000000000000000, -1.000000000000000000 ) ) ;
#3158 = DIRECTION ( 'NONE',  ( -0.000000000000000000, -0.000000000000000000, -1.000000000000000000 ) ) ;
#3159 = ORIENTED_EDGE ( 'NONE', *, *, #5595, .T. ) ;
#3160 = CARTESIAN_POINT ( 'NONE',  ( 11.64999999999996660, 1.426713521006662464E-15, 200.0000000000000000 ) ) ;
#3161 = AXIS2_PLACEMENT_3D ( 'NONE', #4947, #7405, #6836 ) ;
#3162 = APPLICATION_CONTEXT ( 'automotive_design' ) ;
#3163 = CARTESIAN_POINT ( 'NONE',  ( 363.8160267288120622, 19.20325634068194631, -5.642343897998047808 ) ) ;
#3164 = ORIENTED_EDGE ( 'NONE', *, *, #6302, .T. ) ;
#3165 = CARTESIAN_POINT ( 'NONE',  ( 62.50000000000009948, 144.7499999999999147, 130.0000000000000000 ) ) ;
#3166 = AXIS2_PLACEMENT_3D ( 'NONE', #3946, #7040, #4617 ) ;
#3167 = VERTEX_POINT ( 'NONE', #6647 ) ;
#3168 = EDGE_CURVE ( 'NONE', #1999, #6360, #7619, .T. ) ;
#3169 = FACE_OUTER_BOUND ( 'NONE', #589, .T. ) ;
#3170 = DIRECTION ( 'NONE',  ( -0.7071067811865482389, 8.659560562354941486E-17, 0.7071067811865469066 ) ) ;
#3171 = EDGE_CURVE ( 'NONE', #1620, #3797, #1093, .T. ) ;
#3172 = AXIS2_PLACEMENT_3D ( 'NONE', #3499, #7268, #3538 ) ;
#3173 = ORIENTED_EDGE ( 'NONE', *, *, #5870, .T. ) ;
#3174 = ORIENTED_EDGE ( 'NONE', *, *, #3815, .F. ) ;
#3175 = EDGE_CURVE ( 'NONE', #5938, #443, #4295, .T. ) ;
#3176 = ORIENTED_EDGE ( 'NONE', *, *, #1654, .F. ) ;
#3177 = LINE ( 'NONE', #2690, #4703 ) ;
#3178 = ADVANCED_FACE ( 'NONE', ( #3601 ), #7846, .F. ) ;
#3179 = DIRECTION ( 'NONE',  ( 1.000000000000000000, 0.000000000000000000, 0.000000000000000000 ) ) ;
#3180 = LINE ( 'NONE', #81, #6911 ) ;
#3182 = DIRECTION ( 'NONE',  ( -1.000000000000000000, -0.000000000000000000, -0.000000000000000000 ) ) ;
#3181 = VECTOR ( 'NONE', #5044, 1000.000000000000000 ) ;
#3183 = CARTESIAN_POINT ( 'NONE',  ( 0.000000000000000000, 0.000000000000000000, 1.000000000000028644 ) ) ;
#3184 = CIRCLE ( 'NONE', #7910, 74.99999999999995737 ) ;
#3185 = AXIS2_PLACEMENT_3D ( 'NONE', #2020, #2182, #6922 ) ;
#3186 = FACE_OUTER_BOUND ( 'NONE', #2715, .T. ) ;
#3187 = DIRECTION ( 'NONE',  ( 1.000000000000000000, 0.000000000000000000, 0.000000000000000000 ) ) ;
#3188 = DIRECTION ( 'NONE',  ( 0.000000000000000000, 0.000000000000000000, -1.000000000000000000 ) ) ;
#3189 = CARTESIAN_POINT ( 'NONE',  ( 162.4999999999999432, 187.4999999999999716, 0.000000000000000000 ) ) ;
#3190 = VECTOR ( 'NONE', #6594, 1000.000000000000000 ) ;
#3191 = EDGE_LOOP ( 'NONE', ( #879, #4062 ) ) ;
#3192 = AXIS2_PLACEMENT_3D ( 'NONE', #1431, #2807, #7649 ) ;
#3193 = SHAPE_REPRESENTATION_RELATIONSHIP ( 'NONE' , 'NONE' ,  #4527, #958 ) ;
#3194 = ORIENTED_EDGE ( 'NONE', *, *, #2649, .F. ) ;
#3195 = FACE_OUTER_BOUND ( 'NONE', #3405, .T. ) ;
#3196 = CARTESIAN_POINT ( 'NONE',  ( 286.6025403784439050, 75.00000000000002842, 12.50000000000000000 ) ) ;
#3197 = EDGE_CURVE ( 'NONE', #916, #7160, #5364, .T. ) ;
#3198 = FACE_OUTER_BOUND ( 'NONE', #3638, .T. ) ;
#3199 = EDGE_LOOP ( 'NONE', ( #4761, #6917, #426, #1631 ) ) ;
#3200 = DIRECTION ( 'NONE',  ( 0.000000000000000000, -1.000000000000000000, 0.000000000000000000 ) ) ;
#3201 = CIRCLE ( 'NONE', #7300, 12.50000000000001066 ) ;
#3202 = UNCERTAINTY_MEASURE_WITH_UNIT (LENGTH_MEASURE( 1.000000000000000082E-05 ), #1271, 'distance_accuracy_value', 'NONE');
#3203 = ORIENTED_EDGE ( 'NONE', *, *, #168, .T. ) ;
#3204 = CARTESIAN_POINT ( 'NONE',  ( 363.3366216376737157, 19.48763309926589216, -4.514690562563614229 ) ) ;
#3205 = EDGE_LOOP ( 'NONE', ( #3428, #827, #7787 ) ) ;
#3206 = LINE ( 'NONE', #3279, #6991 ) ;
#3207 = ORIENTED_EDGE ( 'NONE', *, *, #2581, .F. ) ;
#3208 = FACE_OUTER_BOUND ( 'NONE', #3365, .T. ) ;
#3209 = CARTESIAN_POINT ( 'NONE',  ( 0.000000000000000000, -25.00000000000000000, 25.00000000000000000 ) ) ;
#3210 = ORIENTED_EDGE ( 'NONE', *, *, #4383, .T. ) ;
#3211 = ADVANCED_FACE ( 'NONE', ( #3522 ), #4117, .T. ) ;
#3212 = ORIENTED_EDGE ( 'NONE', *, *, #6502, .F. ) ;
#3213 = ORIENTED_EDGE ( 'NONE', *, *, #3123, .T. ) ;
#3214 = FACE_OUTER_BOUND ( 'NONE', #4399, .T. ) ;
#3215 = CARTESIAN_POINT ( 'NONE',  ( 379.0967594850577598, -16.13643827696138189, -11.81688677216110861 ) ) ;
#3216 = ORIENTED_EDGE ( 'NONE', *, *, #3327, .T. ) ;
#3217 = LINE ( 'NONE', #2496, #580 ) ;
#3218 = APPLICATION_CONTEXT ( 'automotive_design' ) ;
#3219 = EDGE_CURVE ( 'NONE', #7215, #7248, #4415, .T. ) ;
#3220 = EDGE_CURVE ( 'NONE', #3875, #7818, #3487, .T. ) ;
#3221 = PRODUCT ( 'Bolt3', 'Bolt3', '', ( #2268 ) ) ;
#3222 = DIRECTION ( 'NONE',  ( 1.000000000000000000, 0.000000000000000000, 0.000000000000000000 ) ) ;
#3223 = DIRECTION ( 'NONE',  ( -0.000000000000000000, -0.000000000000000000, -1.000000000000000000 ) ) ;
#3224 = DIRECTION ( 'NONE',  ( 0.000000000000000000, -1.000000000000000000, 0.000000000000000000 ) ) ;
#3225 = CARTESIAN_POINT ( 'NONE',  ( 190.0000000000000000, 12.50000000000000000, -21.65063509461096913 ) ) ;
#3226 = EDGE_CURVE ( 'NONE', #4784, #2186, #2285, .T. ) ;
#3227 = EDGE_LOOP ( 'NONE', ( #4080, #5337, #7788, #4138 ) ) ;
#3228 = PLANE ( 'NONE',  #4079 ) ;
#3229 = EDGE_LOOP ( 'NONE', ( #4919, #751, #3173, #5367 ) ) ;
#3230 = PLANE ( 'NONE',  #4813 ) ;
#3231 = CARTESIAN_POINT ( 'NONE',  ( 0.000000000000000000, 0.000000000000000000, 49.99999999999998579 ) ) ;
#3232 = DIRECTION ( 'NONE',  ( 0.000000000000000000, 0.000000000000000000, -1.000000000000000000 ) ) ;
#3233 = DIRECTION ( 'NONE',  ( 0.000000000000000000, 0.000000000000000000, 1.000000000000000000 ) ) ;
#3234 = VERTEX_POINT ( 'NONE', #4835 ) ;
#3235 = ORIENTED_EDGE ( 'NONE', *, *, #4828, .F. ) ;
#3236 = EDGE_CURVE ( 'NONE', #345, #342, #4713, .T. ) ;
#3237 = CARTESIAN_POINT ( 'NONE',  ( 366.7448740837735954, 17.65381669312412427, -9.419798908014916705 ) ) ;
#3238 = EDGE_LOOP ( 'NONE', ( #986, #7128, #1742, #7247 ) ) ;
#3239 = CARTESIAN_POINT ( 'NONE',  ( 12.50000000000000000, 25.00000000000000355, 7.703719777548943412E-31 ) ) ;
#3240 = ORIENTED_EDGE ( 'NONE', *, *, #7582, .T. ) ;
#3241 = DIRECTION ( 'NONE',  ( 0.000000000000000000, 0.000000000000000000, -1.000000000000000000 ) ) ;
#3242 = CARTESIAN_POINT ( 'NONE',  ( 0.000000000000000000, 0.000000000000000000, 0.000000000000000000 ) ) ;
#3243 = EDGE_LOOP ( 'NONE', ( #7505, #5769, #4946, #2647 ) ) ;
#3244 = CARTESIAN_POINT ( 'NONE',  ( -12.99038105676657651, 1.734723475976807094E-15, 7.500000000000000000 ) ) ;
#3245 = VERTEX_POINT ( 'NONE', #7813 ) ;
#3246 = ORIENTED_EDGE ( 'NONE', *, *, #311, .T. ) ;
#3247 = LINE ( 'NONE', #198, #3557 ) ;
#3248 = LINE ( 'NONE', #315, #6832 ) ;
#3249 = CARTESIAN_POINT ( 'NONE',  ( -24.28095581706361372, 2.657566677470048251E-15, 12.50000000000000000 ) ) ;
#3250 = ORIENTED_EDGE ( 'NONE', *, *, #2987, .T. ) ;
#3251 = DIRECTION ( 'NONE',  ( -1.000000000000000000, 0.000000000000000000, 0.000000000000000000 ) ) ;
#3252 = AXIS2_PLACEMENT_3D ( 'NONE', #7272, #6668, #1172 ) ;
#3253 = CLOSED_SHELL ( 'NONE', ( #2504, #3857, #1157, #5287, #3739, #2459, #3912, #3294, #4144, #7082, #4341, #4098, #5509 ) ) ;
#3254 = CONTEXT_DEPENDENT_SHAPE_REPRESENTATION ( #5257, #6051 ) ;
#3255 = DIRECTION ( 'NONE',  ( 1.000000000000000000, 0.000000000000000000, 0.000000000000000000 ) ) ;
#3256 = FACE_OUTER_BOUND ( 'NONE', #6811, .T. ) ;
#3257 = DIRECTION ( 'NONE',  ( 0.000000000000000000, 0.000000000000000000, 1.000000000000000000 ) ) ;
#3258 = CARTESIAN_POINT ( 'NONE',  ( 375.0000000000000000, 25.00000000000000000, -12.50000000000000000 ) ) ;
#3259 = ADVANCED_FACE ( 'NONE', ( #4791 ), #7214, .F. ) ;
#3260 = ADVANCED_BREP_SHAPE_REPRESENTATION ( '', ( #7010, #5785 ), #5655 ) ;
#3261 = AXIS2_PLACEMENT_3D ( 'NONE', #5125, #7062, #4525 ) ;
#3262 = ADVANCED_FACE ( 'NONE', ( #1110 ), #519, .T. ) ;
#3263 = VECTOR ( 'NONE', #5645, 1000.000000000000114 ) ;
#3264 = VERTEX_POINT ( 'NONE', #3729 ) ;
#3265 = DIRECTION ( 'NONE',  ( 1.000000000000000000, -0.000000000000000000, 0.000000000000000000 ) ) ;
#3266 = EDGE_LOOP ( 'NONE', ( #561, #6662, #6903, #4512 ) ) ;
#3267 = DIRECTION ( 'NONE',  ( 0.000000000000000000, 0.000000000000000000, -1.000000000000000000 ) ) ;
#3268 = CARTESIAN_POINT ( 'NONE',  ( -25.00000000000000000, 0.000000000000000000, 25.00000000000000000 ) ) ;
#3270 = LINE ( 'NONE', #7678, #4912 ) ;
#3269 = CIRCLE ( 'NONE', #3655, 12.50000000000000000 ) ;
#3271 = ADVANCED_FACE ( 'NONE', ( #7450 ), #3045, .T. ) ;
#3272 = AXIS2_PLACEMENT_3D ( 'NONE', #3591, #2386, #5472 ) ;
#3273 = DIRECTION ( 'NONE',  ( 0.000000000000000000, 0.000000000000000000, 1.000000000000000000 ) ) ;
#3274 = ORIENTED_EDGE ( 'NONE', *, *, #4674, .F. ) ;
#3275 = VECTOR ( 'NONE', #5321, 1000.000000000000000 ) ;
#3276 = ORIENTED_EDGE ( 'NONE', *, *, #4634, .T. ) ;
#3277 = DIRECTION ( 'NONE',  ( -0.000000000000000000, 0.000000000000000000, 1.000000000000000000 ) ) ;
#3278 = EDGE_LOOP ( 'NONE', ( #7764, #591 ) ) ;
#3279 = CARTESIAN_POINT ( 'NONE',  ( 182.4759526419164217, -105.3525403784438907, 12.50000000000000000 ) ) ;
#3280 = FACE_BOUND ( 'NONE', #6481, .T. ) ;
#3281 = FACE_OUTER_BOUND ( 'NONE', #6557, .T. ) ;
#3282 = CARTESIAN_POINT ( 'NONE',  ( 0.000000000000000000, 0.000000000000000000, 75.00000000000000000 ) ) ;
#3283 = PRODUCT_DEFINITION_SHAPE ( 'NONE', 'NONE',  #3552 ) ;
#3284 = VERTEX_POINT ( 'NONE', #4351 ) ;
#3285 = AXIS2_PLACEMENT_3D ( 'NONE', #347, #987, #5190 ) ;
#3286 = DIRECTION ( 'NONE',  ( -0.000000000000000000, -0.000000000000000000, 1.000000000000000000 ) ) ;
#3287 = ORIENTED_EDGE ( 'NONE', *, *, #765, .T. ) ;
#3288 = B_SPLINE_CURVE_WITH_KNOTS ( 'NONE', 3,
 ( #5950, #1398, #4815, #1850 ),
 .UNSPECIFIED., .F., .F.,
 ( 4, 4 ),
 ( 0.000000000000000000, 0.003328530869593411285 ),
 .UNSPECIFIED. ) ;
#3289 = ORIENTED_EDGE ( 'NONE', *, *, #6169, .T. ) ;
#3290 = LINE ( 'NONE', #3929, #4964 ) ;
#3291 = CARTESIAN_POINT ( 'NONE',  ( -26.24999999999997158, 177.4999999999999432, 17.50000000000001421 ) ) ;
#3292 = ORIENTED_EDGE ( 'NONE', *, *, #5020, .F. ) ;
#3293 = CARTESIAN_POINT ( 'NONE',  ( 400.0000000000000000, 12.50000000000000000, 12.95183384698871620 ) ) ;
#3294 = ADVANCED_FACE ( 'NONE', ( #7484 ), #5605, .F. ) ;
#3295 = AXIS2_PLACEMENT_3D ( 'NONE', #1573, #4698, #261 ) ;
#3296 = ORIENTED_EDGE ( 'NONE', *, *, #2999, .T. ) ;
#3297 = CIRCLE ( 'NONE', #2281, 25.00000000000000000 ) ;
#3298 = CYLINDRICAL_SURFACE ( 'NONE', #4566, 5.000000000000000888 ) ;
#3299 = DIRECTION ( 'NONE',  ( 1.000000000000000000, 0.000000000000000000, 0.000000000000000000 ) ) ;
#3300 = DIRECTION ( 'NONE',  ( -1.000000000000000000, 0.000000000000000000, 0.000000000000000000 ) ) ;
#3301 = PLANE ( 'NONE',  #3397 ) ;
#3302 = CIRCLE ( 'NONE', #6377, 12.50000000000000000 ) ;
#3303 = VERTEX_POINT ( 'NONE', #1866 ) ;
#3304 = PRODUCT_DEFINITION ( 'UNKNOWN', '', #2582, #4225 ) ;
#3305 = CARTESIAN_POINT ( 'NONE',  ( 124.0868394621949591, 176.6990734970207200, 183.2402661832507249 ) ) ;
#3306 = ORIENTED_EDGE ( 'NONE', *, *, #4528, .F. ) ;
#3307 = CIRCLE ( 'NONE', #5091, 12.50000000000001066 ) ;
#3308 = FACE_OUTER_BOUND ( 'NONE', #4356, .T. ) ;
#3309 = CARTESIAN_POINT ( 'NONE',  ( 12.50000000000000000, -25.00000000000000355, 37.50000000000000000 ) ) ;
#3310 = CARTESIAN_POINT ( 'NONE',  ( -10.82531754730547568, -13.74999999999999822, 7.500000000000000000 ) ) ;
#3311 = EDGE_CURVE ( 'NONE', #2601, #3051, #1731, .T. ) ;
#3312 = DIRECTION ( 'NONE',  ( 0.000000000000000000, 0.000000000000000000, 1.000000000000000000 ) ) ;
#3313 = EDGE_LOOP ( 'NONE', ( #7815, #4023, #4842, #3329 ) ) ;
#3314 = AXIS2_PLACEMENT_3D ( 'NONE', #2761, #6535, #1551 ) ;
#3315 = AXIS2_PLACEMENT_3D ( 'NONE', #6230, #1217, #5634 ) ;
#3316 = EDGE_CURVE ( 'NONE', #3491, #916, #1224, .T. ) ;
#3317 = ORIENTED_EDGE ( 'NONE', *, *, #7315, .F. ) ;
#3318 = ADVANCED_FACE ( 'NONE', ( #5524 ), #746, .F. ) ;
#3319 = DIRECTION ( 'NONE',  ( 1.000000000000000000, 0.000000000000000000, 0.000000000000000000 ) ) ;
#3320 = ORIENTED_EDGE ( 'NONE', *, *, #1303, .F. ) ;
#3321 = DIRECTION ( 'NONE',  ( -0.000000000000000000, -0.000000000000000000, -1.000000000000000000 ) ) ;
#3322 = CARTESIAN_POINT ( 'NONE',  ( 0.000000000000000000, 0.000000000000000000, 97.50000000000000000 ) ) ;
#3323 = EDGE_CURVE ( 'NONE', #4316, #1036, #668, .T. ) ;
#3324 = AXIS2_PLACEMENT_3D ( 'NONE', #6149, #7537, #654 ) ;
#3325 = DIRECTION ( 'NONE',  ( -4.237492460401359023E-16, -1.000000000000000000, 0.000000000000000000 ) ) ;
#3326 = CARTESIAN_POINT ( 'NONE',  ( 3.081487911019577803E-31, 24.99999999999999645, 37.50000000000000711 ) ) ;
#3327 = EDGE_CURVE ( 'NONE', #4382, #5563, #3532, .T. ) ;
#3328 = ADVANCED_FACE ( 'NONE', ( #4911 ), #595, .T. ) ;
#3329 = ORIENTED_EDGE ( 'NONE', *, *, #1600, .F. ) ;
#3330 = CARTESIAN_POINT ( 'NONE',  ( 232.4759526419164786, -18.74999999999998934, 0.000000000000000000 ) ) ;
#3331 = VERTEX_POINT ( 'NONE', #3686 ) ;
#3332 = ORIENTED_EDGE ( 'NONE', *, *, #231, .T. ) ;
#3333 = DIRECTION ( 'NONE',  ( 1.000000000000000000, 0.000000000000000000, -0.000000000000000000 ) ) ;
#3334 = CARTESIAN_POINT ( 'NONE',  ( 0.000000000000000000, 0.000000000000000000, 0.000000000000000000 ) ) ;
#3335 = LINE ( 'NONE', #3887, #7156 ) ;
#3336 = DIRECTION ( 'NONE',  ( 1.000000000000000000, 0.000000000000000000, 0.000000000000000000 ) ) ;
#3337 = ORIENTED_EDGE ( 'NONE', *, *, #6505, .F. ) ;
#3338 = EDGE_CURVE ( 'NONE', #5747, #2966, #1908, .T. ) ;
#3339 = CARTESIAN_POINT ( 'NONE',  ( -49.28095584970496645, -62.29455879088143888, 12.50000000000000000 ) ) ;
#3340 = CARTESIAN_POINT ( 'NONE',  ( 350.0000000000001137, -6.123233995736758985E-15, 0.000000000000000000 ) ) ;
#3341 = DIRECTION ( 'NONE',  ( -1.000000000000000000, 0.000000000000000000, 0.000000000000000000 ) ) ;
#3342 = CARTESIAN_POINT ( 'NONE',  ( 232.4759526419164217, 243.7500000000000000, 12.50000000000000000 ) ) ;
#3343 = DIRECTION ( 'NONE',  ( 0.7071067811865474617, 8.659560562354932858E-17, -0.7071067811865474617 ) ) ;
#3344 = DIRECTION ( 'NONE',  ( -4.789677997474686366E-16, -1.000000000000000000, -0.000000000000000000 ) ) ;
#3345 =( NAMED_UNIT ( * ) SI_UNIT ( $, .STERADIAN. ) SOLID_ANGLE_UNIT ( ) );
#3346 = ORIENTED_EDGE ( 'NONE', *, *, #5324, .T. ) ;
#3347 = DIRECTION ( 'NONE',  ( -1.000000000000000000, 0.000000000000000000, 0.000000000000000000 ) ) ;
#3348 = DIRECTION ( 'NONE',  ( 1.000000000000000000, 0.000000000000000000, 0.000000000000000000 ) ) ;
#3349 = DIRECTION ( 'NONE',  ( 0.000000000000000000, 0.000000000000000000, 1.000000000000000000 ) ) ;
#3350 = CARTESIAN_POINT ( 'NONE',  ( 0.000000000000000000, 0.000000000000000000, 75.00000000000000000 ) ) ;
#3351 = VERTEX_POINT ( 'NONE', #1232 ) ;
#3352 = ORIENTED_EDGE ( 'NONE', *, *, #7315, .T. ) ;
#3353 = PRODUCT_DEFINITION_CONTEXT ( 'detailed design', #6846, 'design' ) ;
#3354 = ORIENTED_EDGE ( 'NONE', *, *, #5784, .F. ) ;
#3355 = CARTESIAN_POINT ( 'NONE',  ( 400.0000000000000000, 20.00000000000000000, 0.000000000000000000 ) ) ;
#3356 = VERTEX_POINT ( 'NONE', #2590 ) ;
#3357 = DIRECTION ( 'NONE',  ( 0.000000000000000000, 1.000000000000000000, 0.000000000000000000 ) ) ;
#3358 = FACE_OUTER_BOUND ( 'NONE', #679, .T. ) ;
#3359 =( NAMED_UNIT ( * ) SI_UNIT ( $, .STERADIAN. ) SOLID_ANGLE_UNIT ( ) );
#3360 = CARTESIAN_POINT ( 'NONE',  ( -27.49999999999989342, 187.4999999999999432, 12.50000000000000000 ) ) ;
#3361 = ADVANCED_FACE ( 'NONE', ( #5029 ), #4872, .T. ) ;
#3362 = ADVANCED_FACE ( 'NONE', ( #5259 ), #4270, .F. ) ;
#3363 = VERTEX_POINT ( 'NONE', #6127 ) ;
#3364 = LINE ( 'NONE', #7573, #4207 ) ;
#3365 = EDGE_LOOP ( 'NONE', ( #7473, #4955 ) ) ;
#3366 = CARTESIAN_POINT ( 'NONE',  ( 412.5000000000000568, 75.00000000000001421, 12.50000000000000000 ) ) ;
#3367 = ORIENTED_EDGE ( 'NONE', *, *, #669, .F. ) ;
#3368 = CARTESIAN_POINT ( 'NONE',  ( -31.24999999999997158, 47.50000000000009237, 17.50000000000001421 ) ) ;
#3369 = LINE ( 'NONE', #3969, #5034 ) ;
#3370 = DIRECTION ( 'NONE',  ( -0.000000000000000000, -0.000000000000000000, -1.000000000000000000 ) ) ;
#3371 = FACE_OUTER_BOUND ( 'NONE', #2316, .T. ) ;
#3372 = B_SPLINE_CURVE_WITH_KNOTS ( 'NONE', 3,
 ( #7544, #2045, #4487, #1437 ),
 .UNSPECIFIED., .F., .F.,
 ( 4, 4 ),
 ( 0.000000000000000000, 0.003328530869593411285 ),
 .UNSPECIFIED. ) ;
#3373 = ORIENTED_EDGE ( 'NONE', *, *, #820, .F. ) ;
#3374 = CARTESIAN_POINT ( 'NONE',  ( 0.000000000000000000, 177.5000000000000000, 130.0000000000000000 ) ) ;
#3375 = CARTESIAN_POINT ( 'NONE',  ( 125.0000000000000000, 0.000000000000000000, 0.000000000000000000 ) ) ;
#3376 = PLANE ( 'NONE',  #5441 ) ;
#3377 = DIRECTION ( 'NONE',  ( -4.789677997474686366E-16, -1.000000000000000000, -0.000000000000000000 ) ) ;
#3378 = CARTESIAN_POINT ( 'NONE',  ( 379.4808720504254325, 16.23886410922228052, 11.67632056536055707 ) ) ;
#3379 = EDGE_CURVE ( 'NONE', #1919, #3284, #7371, .T. ) ;
#3380 = PRESENTATION_LAYER_ASSIGNMENT (  '', '', ( #7743 ) ) ;
#3381 = VECTOR ( 'NONE', #6923, 1000.000000000000000 ) ;
#3382 = CARTESIAN_POINT ( 'NONE',  ( 399.3518360003419048, 12.50000000000000000, 13.85262921941843750 ) ) ;
#3383 = DIRECTION ( 'NONE',  ( -4.788861976296020289E-16, -1.000000000000000000, -1.767773035421031803E-20 ) ) ;
#3384 = ORIENTED_EDGE ( 'NONE', *, *, #2823, .T. ) ;
#3385 = DIRECTION ( 'NONE',  ( 0.000000000000000000, 0.000000000000000000, 1.000000000000000000 ) ) ;
#3386 = CARTESIAN_POINT ( 'NONE',  ( 412.5000000000001137, 1.530808498934191127E-15, 25.00000000000000000 ) ) ;
#3387 = DIRECTION ( 'NONE',  ( 1.000000000000000000, 0.000000000000000000, 0.000000000000000000 ) ) ;
#3388 = FACE_BOUND ( 'NONE', #4479, .T. ) ;
#3389 = VERTEX_POINT ( 'NONE', #6767 ) ;
#3390 = AXIS2_PLACEMENT_3D ( 'NONE', #5818, #6945, #7581 ) ;
#3391 = CIRCLE ( 'NONE', #7234, 12.50000000000001066 ) ;
#3392 = VECTOR ( 'NONE', #3341, 1000.000000000000000 ) ;
#3393 = EDGE_CURVE ( 'NONE', #1872, #5244, #2513, .T. ) ;
#3394 = ORIENTED_EDGE ( 'NONE', *, *, #1728, .T. ) ;
#3395 = VECTOR ( 'NONE', #6289, 1000.000000000000000 ) ;
#3396 = CARTESIAN_POINT ( 'NONE',  ( 0.000000000000000000, 0.000000000000000000, 0.5000000000000004441 ) ) ;
#3397 = AXIS2_PLACEMENT_3D ( 'NONE', #4096, #3938, #2698 ) ;
#3398 = ORIENTED_EDGE ( 'NONE', *, *, #7726, .T. ) ;
#3399 = CARTESIAN_POINT ( 'NONE',  ( -49.28095584970496645, -62.29455879088143888, 12.50000000000000000 ) ) ;
#3400 = DIRECTION ( 'NONE',  ( 4.789677997474685380E-16, 1.000000000000000000, 0.000000000000000000 ) ) ;
#3401 = CYLINDRICAL_SURFACE ( 'NONE', #7366, 12.50000000000000000 ) ;
#3402 = AXIS2_PLACEMENT_3D ( 'NONE', #5559, #1984, #7330 ) ;
#3403 = ORIENTED_EDGE ( 'NONE', *, *, #5117, .F. ) ;
#3404 = DIRECTION ( 'NONE',  ( -0.000000000000000000, -0.000000000000000000, -1.000000000000000000 ) ) ;
#3405 = EDGE_LOOP ( 'NONE', ( #6495, #3462, #6195, #3098 ) ) ;
#3406 = EDGE_CURVE ( 'NONE', #3053, #2333, #6806, .T. ) ;
#3407 = FACE_OUTER_BOUND ( 'NONE', #5292, .T. ) ;
#3408 = VECTOR ( 'NONE', #6574, 1000.000000000000000 ) ;
#3409 = VERTEX_POINT ( 'NONE', #290 ) ;
#3410 = CARTESIAN_POINT ( 'NONE',  ( 162.5000000000000000, 37.50000000000006395, 12.50000000000000000 ) ) ;
#3411 = DIRECTION ( 'NONE',  ( -0.000000000000000000, 0.000000000000000000, 1.000000000000000000 ) ) ;
#3412 = EDGE_CURVE ( 'NONE', #3331, #6641, #5322, .T. ) ;
#3413 = DIRECTION ( 'NONE',  ( 0.000000000000000000, 0.000000000000000000, 1.000000000000000000 ) ) ;
#3414 = EDGE_CURVE ( 'NONE', #5929, #1336, #1474, .T. ) ;
#3415 = ORIENTED_EDGE ( 'NONE', *, *, #6938, .F. ) ;
#3416 = EDGE_CURVE ( 'NONE', #6617, #393, #2741, .T. ) ;
#3417 = PRODUCT ( 'Bolt2', 'Bolt2', '', ( #5951 ) ) ;
#3418 = FACE_OUTER_BOUND ( 'NONE', #4797, .T. ) ;
#3419 = DIRECTION ( 'NONE',  ( -1.000000000000000000, -0.000000000000000000, -0.000000000000000000 ) ) ;
#3421 = DIRECTION ( 'NONE',  ( 1.000000000000000000, 0.000000000000000000, -0.000000000000000000 ) ) ;
#3420=STYLED_ITEM('',(#7941),#4361);
#3422 = CARTESIAN_POINT ( 'NONE',  ( -12.50000000000000000, 0.000000000000000000, 45.00000000000000000 ) ) ;
#3423 = CARTESIAN_POINT ( 'NONE',  ( 386.1818624296773805, 19.20198692117305583, 5.648001166226691794 ) ) ;
#3424 = EDGE_CURVE ( 'NONE', #5200, #7492, #3836, .T. ) ;
#3425 = AXIS2_PLACEMENT_3D ( 'NONE', #1088, #5984, #497 ) ;
#3426 = CARTESIAN_POINT ( 'NONE',  ( 9.381941874331417353, -16.24999999999999645, 0.000000000000000000 ) ) ;
#3427 = CARTESIAN_POINT ( 'NONE',  ( 0.000000000000000000, 0.000000000000000000, 0.000000000000000000 ) ) ;
#3428 = ORIENTED_EDGE ( 'NONE', *, *, #3666, .F. ) ;
#3429 = DIRECTION ( 'NONE',  ( -0.000000000000000000, -0.000000000000000000, -1.000000000000000000 ) ) ;
#3430 = PLANE ( 'NONE',  #7795 ) ;
#3431 = CARTESIAN_POINT ( 'NONE',  ( 0.000000000000000000, 187.4999999999999432, 12.50000000000000000 ) ) ;
#3432 = CARTESIAN_POINT ( 'NONE',  ( 125.0000000000000000, 0.000000000000000000, 0.000000000000000000 ) ) ;
#3433 = ORIENTED_EDGE ( 'NONE', *, *, #7478, .F. ) ;
#3434 = CIRCLE ( 'NONE', #5354, 25.00000000000000000 ) ;
#3435 = ORIENTED_EDGE ( 'NONE', *, *, #7115, .T. ) ;
#3436 = EDGE_LOOP ( 'NONE', ( #7512, #4705 ) ) ;
#3437 = PRESENTATION_LAYER_ASSIGNMENT (  '', '', ( #6768 ) ) ;
#3438 = VECTOR ( 'NONE', #3724, 1000.000000000000000 ) ;
#3439 = DIRECTION ( 'NONE',  ( 0.000000000000000000, 0.000000000000000000, 1.000000000000000000 ) ) ;
#3440 = ORIENTED_EDGE ( 'NONE', *, *, #669, .T. ) ;
#3441 = ADVANCED_FACE ( 'NONE', ( #4574 ), #7034, .F. ) ;
#3442 = CARTESIAN_POINT ( 'NONE',  ( 412.4999999999998863, 82.50000000000004263, 155.0000000000000000 ) ) ;
#3443 = CARTESIAN_POINT ( 'NONE',  ( 0.000000000000000000, 0.000000000000000000, 0.000000000000000000 ) ) ;
#3444 = VERTEX_POINT ( 'NONE', #4097 ) ;
#3445 = FILL_AREA_STYLE ('',( #5320 ) ) ;
#3446 = DIRECTION ( 'NONE',  ( 1.000000000000000000, 0.000000000000000000, 0.000000000000000000 ) ) ;
#3447 = AXIS2_PLACEMENT_3D ( 'NONE', #3959, #5613, #113 ) ;
#3448 = AXIS2_PLACEMENT_3D ( 'NONE', #583, #6192, #3714 ) ;
#3449 = ORIENTED_EDGE ( 'NONE', *, *, #1545, .F. ) ;
#3450 = CARTESIAN_POINT ( 'NONE',  ( 12.50000000000000000, 4.382085397712380109E-15, -35.78244274809159720 ) ) ;
#3451 = VERTEX_POINT ( 'NONE', #6513 ) ;
#3452 = CIRCLE ( 'NONE', #2949, 37.50000000000000000 ) ;
#3453 = CARTESIAN_POINT ( 'NONE',  ( 42.50000000000000711, 182.5000000000000000, 12.50000000000000000 ) ) ;
#3454 = CIRCLE ( 'NONE', #513, 17.50000000000000355 ) ;
#3455 = ORIENTED_EDGE ( 'NONE', *, *, #6480, .T. ) ;
#3456 = DIRECTION ( 'NONE',  ( 1.000000000000000000, 0.000000000000000000, 0.000000000000000000 ) ) ;
#3457 = DIRECTION ( 'NONE',  ( 1.000000000000000000, 0.000000000000000000, 0.000000000000000000 ) ) ;
#3458 = CARTESIAN_POINT ( 'NONE',  ( -7.184516996212029076E-14, 149.9999999999998295, 5.000000000000000000 ) ) ;
#3459 = DIRECTION ( 'NONE',  ( 0.000000000000000000, 0.000000000000000000, 1.000000000000000000 ) ) ;
#3460 = CIRCLE ( 'NONE', #5523, 12.50000000000000000 ) ;
#3461 = PRODUCT_RELATED_PRODUCT_CATEGORY ( 'part', '', ( #6933 ) ) ;
#3462 = ORIENTED_EDGE ( 'NONE', *, *, #7079, .F. ) ;
#3463 = ORIENTED_EDGE ( 'NONE', *, *, #4478, .T. ) ;
#3464 = PLANE ( 'NONE',  #988 ) ;
#3465 = DIRECTION ( 'NONE',  ( 1.000000000000000000, 0.000000000000000000, 0.000000000000000000 ) ) ;
#3466 = LINE ( 'NONE', #2304, #2341 ) ;
#3467 = DIRECTION ( 'NONE',  ( 0.000000000000000000, -1.000000000000000000, 0.000000000000000000 ) ) ;
#3468 = CARTESIAN_POINT ( 'NONE',  ( 75.00000000000000000, 10.56842436860067735, 0.000000000000000000 ) ) ;
#3469 = ADVANCED_FACE ( 'NONE', ( #2218 ), #5792, .T. ) ;
#3470 = EDGE_CURVE ( 'NONE', #1036, #3550, #5454, .T. ) ;
#3471 = CARTESIAN_POINT ( 'NONE',  ( -24.28095581706361727, -30.59582894744887582, 12.50000000000000000 ) ) ;
#3472 = SHAPE_DEFINITION_REPRESENTATION ( #6870, #6292 ) ;
#3473 = ORIENTED_EDGE ( 'NONE', *, *, #6012, .T. ) ;
#3474 = CARTESIAN_POINT ( 'NONE',  ( 25.00000000000000000, 25.00000000000000000, 0.000000000000000000 ) ) ;
#3475 = CARTESIAN_POINT ( 'NONE',  ( -31.24999999999997158, 0.000000000000000000, 17.50000000000001421 ) ) ;
#3476 = CYLINDRICAL_SURFACE ( 'NONE', #5301, 25.00000000000000000 ) ;
#3477 = FACE_BOUND ( 'NONE', #5533, .T. ) ;
#3478 = VERTEX_POINT ( 'NONE', #4694 ) ;
#3479 = VERTEX_POINT ( 'NONE', #7113 ) ;
#3480 = EDGE_LOOP ( 'NONE', ( #2250, #4398, #25, #7064, #5731, #7426, #3435, #6441, #7746, #4344, #7223, #7363, #4468 ) ) ;
#3481 = ORIENTED_EDGE ( 'NONE', *, *, #6756, .F. ) ;
#3482 = FILL_AREA_STYLE ('',( #1031 ) ) ;
#3483 = DIRECTION ( 'NONE',  ( -1.000000000000000000, 0.000000000000000000, 0.000000000000000000 ) ) ;
#3484 = AXIS2_PLACEMENT_3D ( 'NONE', #4578, #6393, #5177 ) ;
#3485 = VERTEX_POINT ( 'NONE', #4059 ) ;
#3486 = FILL_AREA_STYLE_COLOUR ( '', #1007 ) ;
#3487 = LINE ( 'NONE', #2886, #3275 ) ;
#3488 = EDGE_CURVE ( 'NONE', #5142, #1620, #6429, .T. ) ;
#3489 = ORIENTED_EDGE ( 'NONE', *, *, #2806, .F. ) ;
#3490 = DIRECTION ( 'NONE',  ( -1.000000000000000000, 0.000000000000000000, 0.000000000000000000 ) ) ;
#3491 = VERTEX_POINT ( 'NONE', #416 ) ;
#3492 = DIRECTION ( 'NONE',  ( -0.000000000000000000, 0.000000000000000000, 1.000000000000000000 ) ) ;
#3493 = VERTEX_POINT ( 'NONE', #2782 ) ;
#3494 = CARTESIAN_POINT ( 'NONE',  ( 162.5000000000000000, 112.5000000000000142, 12.50000000000000000 ) ) ;
#3495 = CARTESIAN_POINT ( 'NONE',  ( 296.6025403784439050, 0.000000000000000000, 0.000000000000000000 ) ) ;
#3496 = EDGE_CURVE ( 'NONE', #6926, #6174, #4163, .T. ) ;
#3497 = EDGE_LOOP ( 'NONE', ( #6730, #6218, #2764, #6291 ) ) ;
#3498 = ORIENTED_EDGE ( 'NONE', *, *, #7702, .T. ) ;
#3499 = CARTESIAN_POINT ( 'NONE',  ( 0.000000000000000000, 0.000000000000000000, 0.000000000000000000 ) ) ;
#3500 = DIRECTION ( 'NONE',  ( -1.000000000000000000, 0.000000000000000000, 0.000000000000000000 ) ) ;
#3501 = DIRECTION ( 'NONE',  ( 1.000000000000000000, 0.000000000000000000, 0.000000000000000000 ) ) ;
#3502 = DIRECTION ( 'NONE',  ( 0.000000000000000000, 0.000000000000000000, -1.000000000000000000 ) ) ;
#3503 = CARTESIAN_POINT ( 'NONE',  ( 0.000000000000000000, 0.000000000000000000, 2.500000000000085265 ) ) ;
#3504 = CARTESIAN_POINT ( 'NONE',  ( -25.00000000000000000, 0.000000000000000000, 0.000000000000000000 ) ) ;
#3505 = ORIENTED_EDGE ( 'NONE', *, *, #4734, .T. ) ;
#3506 = AXIS2_PLACEMENT_3D ( 'NONE', #3558, #4832, #4075 ) ;
#3507 = EDGE_CURVE ( 'NONE', #968, #3409, #388, .T. ) ;
#3508 = FILL_AREA_STYLE ('',( #2344 ) ) ;
#3509 = DIRECTION ( 'NONE',  ( 1.000000000000000000, 0.000000000000000000, 0.000000000000000000 ) ) ;
#3510 = FACE_OUTER_BOUND ( 'NONE', #3692, .T. ) ;
#3511 = FACE_OUTER_BOUND ( 'NONE', #7877, .T. ) ;
#3512 = ORIENTED_EDGE ( 'NONE', *, *, #4046, .F. ) ;
#3513 = EDGE_CURVE ( 'NONE', #5007, #7081, #1855, .T. ) ;
#3514 = AXIS2_PLACEMENT_3D ( 'NONE', #1811, #576, #5463 ) ;
#3515 = CONICAL_SURFACE ( 'NONE', #1845, 31.78244274809162562, 0.7853981633974447263 ) ;
#3516 = ORIENTED_EDGE ( 'NONE', *, *, #6747, .T. ) ;
#3517 = EDGE_CURVE ( 'NONE', #3564, #2186, #6587, .T. ) ;
#3518 = ORIENTED_EDGE ( 'NONE', *, *, #7912, .T. ) ;
#3519 = CARTESIAN_POINT ( 'NONE',  ( 13.00000000000000178, 0.000000000000000000, 2.168404344971008868E-16 ) ) ;
#3520 = AXIS2_PLACEMENT_3D ( 'NONE', #3548, #5995, #4413 ) ;
#3521 = ORIENTED_EDGE ( 'NONE', *, *, #4531, .F. ) ;
#3522 = FACE_OUTER_BOUND ( 'NONE', #749, .T. ) ;
#3523 = VECTOR ( 'NONE', #6893, 1000.000000000000000 ) ;
#3524 = VERTEX_POINT ( 'NONE', #5385 ) ;
#3525 = AXIS2_PLACEMENT_3D ( 'NONE', #1049, #2821, #7708 ) ;
#3526 = EDGE_CURVE ( 'NONE', #2477, #3534, #2763, .T. ) ;
#3527 = DIRECTION ( 'NONE',  ( 0.8660254037844385966, 0.5000000000000003331, -0.000000000000000000 ) ) ;
#3528 = ORIENTED_EDGE ( 'NONE', *, *, #4550, .F. ) ;
#3529 = CARTESIAN_POINT ( 'NONE',  ( 182.4759526419164217, -105.3525403784438907, 0.000000000000000000 ) ) ;
#3530 = EDGE_LOOP ( 'NONE', ( #4481, #2118, #1243, #5021 ) ) ;
#3531 = DIRECTION ( 'NONE',  ( -0.000000000000000000, -0.000000000000000000, 1.000000000000000000 ) ) ;
#3532 = CIRCLE ( 'NONE', #62, 65.50000000000000000 ) ;
#3533 = CYLINDRICAL_SURFACE ( 'NONE', #6856, 12.49999999999999467 ) ;
#3534 = VERTEX_POINT ( 'NONE', #577 ) ;
#3535 = AXIS2_PLACEMENT_3D ( 'NONE', #6247, #4473, #1389 ) ;
#3536 = ORIENTED_EDGE ( 'NONE', *, *, #4478, .F. ) ;
#3537 = EDGE_CURVE ( 'NONE', #3491, #2126, #2377, .T. ) ;
#3538 = DIRECTION ( 'NONE',  ( 1.000000000000000000, 0.000000000000000000, 0.000000000000000000 ) ) ;
#3539 = CARTESIAN_POINT ( 'NONE',  ( 12.50000000000000355, 0.000000000000000000, -25.00000000000000000 ) ) ;
#3540 = CARTESIAN_POINT ( 'NONE',  ( 42.50000000000000000, 47.50000000000003553, 12.50000000000000000 ) ) ;
#3541 = CYLINDRICAL_SURFACE ( 'NONE', #3642, 32.75000000000001421 ) ;
#3542 = CIRCLE ( 'NONE', #7629, 32.75000000000000000 ) ;
#3543 = DIRECTION ( 'NONE',  ( 0.000000000000000000, -0.000000000000000000, -1.000000000000000000 ) ) ;
#3544 = LINE ( 'NONE', #3426, #2941 ) ;
#3545 = VECTOR ( 'NONE', #5677, 1000.000000000000000 ) ;
#3546 = ORIENTED_EDGE ( 'NONE', *, *, #6938, .T. ) ;
#3547 = CARTESIAN_POINT ( 'NONE',  ( 32.53766565774834163, -18.78563002630307111, 0.000000000000000000 ) ) ;
#3548 = CARTESIAN_POINT ( 'NONE',  ( 0.000000000000000000, 25.00000000000000000, 25.00000000000000000 ) ) ;
#3549 = DIRECTION ( 'NONE',  ( -0.000000000000000000, -0.000000000000000000, -1.000000000000000000 ) ) ;
#3550 = VERTEX_POINT ( 'NONE', #1771 ) ;
#3551 = AXIS2_PLACEMENT_3D ( 'NONE', #7028, #3894, #6342 ) ;
#3552 = PRODUCT_DEFINITION ( 'UNKNOWN', '', #1684, #2873 ) ;
#3553 = EDGE_LOOP ( 'NONE', ( #4559, #2875, #3276, #2646 ) ) ;
#3554 = EDGE_CURVE ( 'NONE', #5735, #3493, #4217, .T. ) ;
#3555 = EDGE_LOOP ( 'NONE', ( #524, #6760 ) ) ;
#3556 = DIRECTION ( 'NONE',  ( 0.000000000000000000, 1.000000000000000000, 0.000000000000000000 ) ) ;
#3557 = VECTOR ( 'NONE', #3885, 1000.000000000000000 ) ;
#3558 = CARTESIAN_POINT ( 'NONE',  ( 25.71904415029483459, 19.40417101989674009, 0.000000000000000000 ) ) ;
#3559 = ORIENTED_EDGE ( 'NONE', *, *, #2858, .F. ) ;
#3560 = CARTESIAN_POINT ( 'NONE',  ( 46.25000000000002842, 112.5000000000000142, 195.4980915752512658 ) ) ;
#3561 = VECTOR ( 'NONE', #6175, 1000.000000000000000 ) ;
#3562 = EDGE_CURVE ( 'NONE', #5728, #6174, #6068, .T. ) ;
#3563 = CIRCLE ( 'NONE', #4576, 12.49999999999999467 ) ;
#3564 = VERTEX_POINT ( 'NONE', #1210 ) ;
#3565 = EDGE_CURVE ( 'NONE', #3864, #6728, #328, .T. ) ;
#3566 = CARTESIAN_POINT ( 'NONE',  ( 0.000000000000000000, 0.000000000000000000, 45.00000000000000000 ) ) ;
#3567 = EDGE_LOOP ( 'NONE', ( #7018, #6372 ) ) ;
#3568 = CARTESIAN_POINT ( 'NONE',  ( 363.8181375703225626, -19.20198692117305583, 5.648001166226691794 ) ) ;
#3569 = ORIENTED_EDGE ( 'NONE', *, *, #6409, .T. ) ;
#3570 = AXIS2_PLACEMENT_3D ( 'NONE', #2703, #7555, #4417 ) ;
#3571 = FACE_OUTER_BOUND ( 'NONE', #6042, .T. ) ;
#3572 = CARTESIAN_POINT ( 'NONE',  ( 12.50000000000000000, 1.530808498934191521E-15, 12.50000000000000000 ) ) ;
#3573 = ADVANCED_FACE ( 'NONE', ( #5245 ), #7056, .T. ) ;
#3574 = ORIENTED_EDGE ( 'NONE', *, *, #237, .T. ) ;
#3575 = CIRCLE ( 'NONE', #752, 31.24999999999998579 ) ;
#3576 = TOROIDAL_SURFACE ( 'NONE', #1393, 13.00000000000000178, 0.5000000000000000000 ) ;
#3577 = VERTEX_POINT ( 'NONE', #7139 ) ;
#3578 = LINE ( 'NONE', #1767, #2008 ) ;
#3579 = DIRECTION ( 'NONE',  ( -0.000000000000000000, -0.000000000000000000, -1.000000000000000000 ) ) ;
#3580 = LINE ( 'NONE', #3540, #3783 ) ;
#3581 = DIRECTION ( 'NONE',  ( 0.7071067811865500152, 8.659560562354903276E-17, 0.7071067811865451302 ) ) ;
#3582 = VECTOR ( 'NONE', #7181, 1000.000000000000000 ) ;
#3583 = AXIS2_PLACEMENT_3D ( 'NONE', #5942, #2946, #2903 ) ;
#3584 = CARTESIAN_POINT ( 'NONE',  ( 375.4248592744880852, 15.61249499599599666, -12.50000000000000000 ) ) ;
#3585 = EDGE_CURVE ( 'NONE', #2101, #2637, #715, .T. ) ;
#3586 = CARTESIAN_POINT ( 'NONE',  ( 52.50000000000000711, 113.0000000000000426, 130.0000000000000000 ) ) ;
#3587 = SHAPE_DEFINITION_REPRESENTATION ( #6290, #1772 ) ;
#3588 = DIRECTION ( 'NONE',  ( 0.000000000000000000, 0.000000000000000000, -1.000000000000000000 ) ) ;
#3589 = DIRECTION ( 'NONE',  ( 1.000000000000000000, 0.000000000000000000, 0.000000000000000000 ) ) ;
#3590 = CARTESIAN_POINT ( 'NONE',  ( 375.0000000000000000, 25.00000000000000000, 3.061616997868383043E-15 ) ) ;
#3591 = CARTESIAN_POINT ( 'NONE',  ( 412.4999999999998863, 137.4999999999999716, 17.49999999999998934 ) ) ;
#3592 = EDGE_LOOP ( 'NONE', ( #6539, #2317, #6143, #1406, #738, #3772, #7856, #6876, #7477, #977, #2291, #1275, #7536 ) ) ;
#3593 = VERTEX_POINT ( 'NONE', #1040 ) ;
#3594 = ORIENTED_EDGE ( 'NONE', *, *, #1226, .T. ) ;
#3595 = ORIENTED_EDGE ( 'NONE', *, *, #7679, .T. ) ;
#3596 = DIRECTION ( 'NONE',  ( -1.000000000000000000, 0.000000000000000000, 0.000000000000000000 ) ) ;
#3597 = CYLINDRICAL_SURFACE ( 'NONE', #742, 5.000000000000000000 ) ;
#3598 = DIRECTION ( 'NONE',  ( -1.000000000000000000, -0.000000000000000000, -0.000000000000000000 ) ) ;
#3599 = DIRECTION ( 'NONE',  ( -1.000000000000000000, -0.000000000000000000, -0.000000000000000000 ) ) ;
#3600 = ORIENTED_EDGE ( 'NONE', *, *, #7291, .F. ) ;
#3601 = FACE_OUTER_BOUND ( 'NONE', #5246, .T. ) ;
#3602 = ORIENTED_EDGE ( 'NONE', *, *, #7686, .T. ) ;
#3603 = DIRECTION ( 'NONE',  ( 0.000000000000000000, 0.000000000000000000, -1.000000000000000000 ) ) ;
#3605 = ORIENTED_EDGE ( 'NONE', *, *, #276, .T. ) ;
#3604 = AXIS2_PLACEMENT_3D ( 'NONE', #4471, #1466, #7526 ) ;
#3606 = CARTESIAN_POINT ( 'NONE',  ( 365.6048426980225372, -18.21476284106545052, -8.283543559714008353 ) ) ;
#3607 = ORIENTED_EDGE ( 'NONE', *, *, #4728, .T. ) ;
#3608 = EDGE_CURVE ( 'NONE', #4076, #6800, #1992, .T. ) ;
#3609 = FACE_BOUND ( 'NONE', #5698, .T. ) ;
#3610 = CARTESIAN_POINT ( 'NONE',  ( -25.00000000000000000, 24.99999999999999289, 50.00000000000000000 ) ) ;
#3611 = EDGE_CURVE ( 'NONE', #1117, #1583, #5854, .T. ) ;
#3612 = AXIS2_PLACEMENT_3D ( 'NONE', #6591, #2220, #1095 ) ;
#3613 = EDGE_LOOP ( 'NONE', ( #2440, #4322, #7734, #876 ) ) ;
#3614 = ORIENTED_EDGE ( 'NONE', *, *, #5118, .F. ) ;
#3615 = ADVANCED_FACE ( 'NONE', ( #2326 ), #4721, .F. ) ;
#3616 = CARTESIAN_POINT ( 'NONE',  ( 380.6144942247103131, -16.57606561041850313, 11.19744344920339962 ) ) ;
#3617 = AXIS2_PLACEMENT_3D ( 'NONE', #499, #7228, #1014 ) ;
#3618 = CARTESIAN_POINT ( 'NONE',  ( 0.000000000000000000, 0.000000000000000000, 0.000000000000000000 ) ) ;
#3619 = CARTESIAN_POINT ( 'NONE',  ( -12.99038105676657651, 1.734723475976807094E-15, 7.500000000000000000 ) ) ;
#3620 = LINE ( 'NONE', #2532, #5275 ) ;
#3621 = CARTESIAN_POINT ( 'NONE',  ( 6.602357126051254174E-16, 3.892226678053441094E-15, 31.78244274809162562 ) ) ;
#3622 = DIRECTION ( 'NONE',  ( -0.000000000000000000, 0.000000000000000000, 1.000000000000000000 ) ) ;
#3623 = DIRECTION ( 'NONE',  ( 1.000000000000000000, 0.000000000000000000, 0.000000000000000000 ) ) ;
#3624 = APPLICATION_PROTOCOL_DEFINITION ( 'draft international standard', 'automotive_design', 1998, #3012 ) ;
#3625 = CARTESIAN_POINT ( 'NONE',  ( 326.6025403784438481, 150.0000000000000568, 125.0000000000000000 ) ) ;
#3626 = DIRECTION ( 'NONE',  ( 0.000000000000000000, -1.000000000000000000, 0.000000000000000000 ) ) ;
#3627 = DIRECTION ( 'NONE',  ( -0.000000000000000000, -0.000000000000000000, -1.000000000000000000 ) ) ;
#3628 =( REPRESENTATION_RELATIONSHIP ('NONE','NONE', #6292, #6180 ) REPRESENTATION_RELATIONSHIP_WITH_TRANSFORMATION ( #6114 )SHAPE_REPRESENTATION_RELATIONSHIP( ) );
#3629 = EDGE_CURVE ( 'NONE', #5360, #5569, #1233, .T. ) ;
#3630 = DIRECTION ( 'NONE',  ( 1.000000000000000000, 0.000000000000000000, 0.000000000000000000 ) ) ;
#3631 = ORIENTED_EDGE ( 'NONE', *, *, #6771, .T. ) ;
#3632 = ORIENTED_EDGE ( 'NONE', *, *, #4092, .T. ) ;
#3633 = DIRECTION ( 'NONE',  ( -1.000000000000000000, -2.960594732333750117E-15, 0.000000000000000000 ) ) ;
#3634 = CARTESIAN_POINT ( 'NONE',  ( 337.5000000000000568, -6.123233995736758985E-15, 25.00000000000000000 ) ) ;
#3635 = CARTESIAN_POINT ( 'NONE',  ( 17.32050807568877104, 2.500000000000000444, 0.000000000000000000 ) ) ;
#3636 = EDGE_CURVE ( 'NONE', #7566, #846, #442, .T. ) ;
#3637 = DIRECTION ( 'NONE',  ( 0.000000000000000000, -0.000000000000000000, 1.000000000000000000 ) ) ;
#3638 = EDGE_LOOP ( 'NONE', ( #2164, #4874, #4741, #1667 ) ) ;
#3639 = AXIS2_PLACEMENT_3D ( 'NONE', #585, #3035, #3674 ) ;
#3640 = DIRECTION ( 'NONE',  ( 0.4585571717133497538, 0.8886649088774990490, -0.000000000000000000 ) ) ;
#3641 = ORIENTED_EDGE ( 'NONE', *, *, #2180, .F. ) ;
#3642 = AXIS2_PLACEMENT_3D ( 'NONE', #4856, #3663, #2985 ) ;
#3643 = DIRECTION ( 'NONE',  ( 1.000000000000000000, 0.000000000000000000, 0.000000000000000000 ) ) ;
#3644 = VERTEX_POINT ( 'NONE', #312 ) ;
#3645 = AXIS2_PLACEMENT_3D ( 'NONE', #6608, #1673, #6566 ) ;
#3646 = CARTESIAN_POINT ( 'NONE',  ( 365.0969724145188025, -18.48453940650270866, -7.670107965951052265 ) ) ;
#3647 = ORIENTED_EDGE ( 'NONE', *, *, #7243, .F. ) ;
#3648 = DIRECTION ( 'NONE',  ( -4.789677997474686366E-16, -1.000000000000000000, -0.000000000000000000 ) ) ;
#3649 = DIRECTION ( 'NONE',  ( -1.000000000000000000, 0.000000000000000000, 0.000000000000000000 ) ) ;
#3650 = AXIS2_PLACEMENT_3D ( 'NONE', #5858, #5250, #1527 ) ;
#3651 = AXIS2_PLACEMENT_3D ( 'NONE', #1941, #3312, #4381 ) ;
#3652 = ORIENTED_EDGE ( 'NONE', *, *, #5473, .T. ) ;
#3653 = EDGE_CURVE ( 'NONE', #4754, #5349, #204, .T. ) ;
#3654 = ORIENTED_EDGE ( 'NONE', *, *, #3338, .T. ) ;
#3655 = AXIS2_PLACEMENT_3D ( 'NONE', #5408, #1801, #4244 ) ;
#3656 = EDGE_CURVE ( 'NONE', #7589, #792, #4638, .T. ) ;
#3657 = DIRECTION ( 'NONE',  ( 1.000000000000000000, 0.000000000000000000, 0.000000000000000000 ) ) ;
#3658 = AXIS2_PLACEMENT_3D ( 'NONE', #7803, #658, #510 ) ;
#3659 = VECTOR ( 'NONE', #2337, 1000.000000000000000 ) ;
#3660 = DIRECTION ( 'NONE',  ( -0.000000000000000000, 0.000000000000000000, 1.000000000000000000 ) ) ;
#3661 = DIRECTION ( 'NONE',  ( 0.000000000000000000, 0.000000000000000000, 1.000000000000000000 ) ) ;
#3662 = DIRECTION ( 'NONE',  ( -0.000000000000000000, -0.000000000000000000, -1.000000000000000000 ) ) ;
#3663 = DIRECTION ( 'NONE',  ( -1.000000000000000000, 4.270088556250607616E-16, -0.000000000000000000 ) ) ;
#3664 = CARTESIAN_POINT ( 'NONE',  ( 383.2505588518543505, 17.65634310857833356, -9.398786704980601314 ) ) ;
#3665 = AXIS2_PLACEMENT_3D ( 'NONE', #2322, #1676, #4078 ) ;
#3666 = EDGE_CURVE ( 'NONE', #6766, #2057, #2767, .T. ) ;
#3667 = EDGE_CURVE ( 'NONE', #698, #1300, #5716, .T. ) ;
#3668 = DIRECTION ( 'NONE',  ( 1.000000000000000000, -0.000000000000000000, -0.000000000000000000 ) ) ;
#3669 = CONTEXT_DEPENDENT_SHAPE_REPRESENTATION ( #7320, #1485 ) ;
#3670 = CARTESIAN_POINT ( 'NONE',  ( -12.50000000000000000, 0.000000000000000000, -12.50000000000000000 ) ) ;
#3671 = CARTESIAN_POINT ( 'NONE',  ( 20.00000000000000000, 2.449293598294706513E-15, 47.50000000000000000 ) ) ;
#3673 = DIRECTION ( 'NONE',  ( 0.000000000000000000, -0.000000000000000000, 1.000000000000000000 ) ) ;
#3672 = CIRCLE ( 'NONE', #4681, 5.000000000000000888 ) ;
#3674 = DIRECTION ( 'NONE',  ( -1.000000000000000000, 0.000000000000000000, 0.000000000000000000 ) ) ;
#3675 = EDGE_CURVE ( 'NONE', #4927, #1, #596, .T. ) ;
#3676 = EDGE_CURVE ( 'NONE', #3245, #1578, #6736, .T. ) ;
#3677 = AXIS2_PLACEMENT_3D ( 'NONE', #6005, #3116, #3267 ) ;
#3678 =( NAMED_UNIT ( * ) PLANE_ANGLE_UNIT ( ) SI_UNIT ( $, .RADIAN. ) );
#3679 = EDGE_LOOP ( 'NONE', ( #6049, #2040 ) ) ;
#3680 = DIRECTION ( 'NONE',  ( -1.000000000000000000, -0.000000000000000000, -0.000000000000000000 ) ) ;
#3681 = DIRECTION ( 'NONE',  ( 0.000000000000000000, -1.000000000000000000, 0.000000000000000000 ) ) ;
#3682 = DIRECTION ( 'NONE',  ( -0.4463453945640545872, 2.055455305587023282E-16, 0.8948607650084221543 ) ) ;
#3683 = DIRECTION ( 'NONE',  ( -0.5000000000000003331, 0.8660254037844384856, 0.000000000000000000 ) ) ;
#3684 = VERTEX_POINT ( 'NONE', #7096 ) ;
#3685 = VECTOR ( 'NONE', #5599, 1000.000000000000000 ) ;
#3686 = CARTESIAN_POINT ( 'NONE',  ( 0.7190441502950353225, 87.70544117646394966, 12.50000000000000000 ) ) ;
#3687 = PRODUCT_DEFINITION_SHAPE ( 'NONE', 'NONE',  #7927 ) ;
#3688 = ORIENTED_EDGE ( 'NONE', *, *, #2988, .F. ) ;
#3689 = ADVANCED_FACE ( 'NONE', ( #3407 ), #356, .T. ) ;
#3690 = AXIS2_PLACEMENT_3D ( 'NONE', #3339, #2819, #5788 ) ;
#3691 = CARTESIAN_POINT ( 'NONE',  ( 364.8773838277618324, 18.60597098153023055, -7.344632615169738088 ) ) ;
#3692 = EDGE_LOOP ( 'NONE', ( #4518, #1267, #667, #5100, #2520 ) ) ;
#3693 = CARTESIAN_POINT ( 'NONE',  ( 364.2066703214222230, -18.97948036624223533, -6.318259067610828339 ) ) ;
#3694 = ORIENTED_EDGE ( 'NONE', *, *, #2085, .T. ) ;
#3695 = FACE_BOUND ( 'NONE', #1360, .T. ) ;
#3696 = CYLINDRICAL_SURFACE ( 'NONE', #2104, 12.50000000000000000 ) ;
#3697 = VECTOR ( 'NONE', #2453, 1000.000000000000000 ) ;
#3698 = ORIENTED_EDGE ( 'NONE', *, *, #2623, .T. ) ;
#3699 = ORIENTED_EDGE ( 'NONE', *, *, #6258, .F. ) ;
#3700 = VECTOR ( 'NONE', #200, 1000.000000000000000 ) ;
#3701 = AXIS2_PLACEMENT_3D ( 'NONE', #402, #5286, #2353 ) ;
#3702 = EDGE_LOOP ( 'NONE', ( #6853, #4757, #3740, #2889 ) ) ;
#3703 = DIRECTION ( 'NONE',  ( 0.8948607650084221543, -4.286094916964204981E-16, 0.4463453945640545317 ) ) ;
#3704 = CARTESIAN_POINT ( 'NONE',  ( 387.5008780787119349, -20.00054879841449562, 0.3963588355767777571 ) ) ;
#3705 = FACE_OUTER_BOUND ( 'NONE', #7210, .T. ) ;
#3706 = LINE ( 'NONE', #4292, #802 ) ;
#3707 = CARTESIAN_POINT ( 'NONE',  ( 0.000000000000000000, 0.000000000000000000, 1.000000000000028644 ) ) ;
#3708 = AXIS2_PLACEMENT_3D ( 'NONE', #2196, #991, #7051 ) ;
#3709 = VECTOR ( 'NONE', #7357, 1000.000000000000000 ) ;
#3710 = DIRECTION ( 'NONE',  ( 1.000000000000000000, -0.000000000000000000, -0.000000000000000000 ) ) ;
#3711 = APPLICATION_PROTOCOL_DEFINITION ( 'draft international standard', 'automotive_design', 1998, #3162 ) ;
#3712 = VECTOR ( 'NONE', #6294, 1000.000000000000000 ) ;
#3713 = CARTESIAN_POINT ( 'NONE',  ( 325.0000000000000000, 0.000000000000000000, 0.000000000000000000 ) ) ;
#3714 = DIRECTION ( 'NONE',  ( 0.000000000000000000, 0.000000000000000000, 1.000000000000000000 ) ) ;
#3715 = CIRCLE ( 'NONE', #2034, 25.00000000000000000 ) ;
#3716 = CARTESIAN_POINT ( 'NONE',  ( 38.21904415029501934, 62.70544120911855401, 0.000000000000000000 ) ) ;
#3717 = CARTESIAN_POINT ( 'NONE',  ( -37.49999999999995026, 47.50000000000009237, 5.000000000000000000 ) ) ;
#3718 = EDGE_CURVE ( 'NONE', #6450, #6891, #998, .T. ) ;
#3719 = ADVANCED_FACE ( 'NONE', ( #5932 ), #7736, .F. ) ;
#3720 = ORIENTED_EDGE ( 'NONE', *, *, #6076, .F. ) ;
#3721 = VERTEX_POINT ( 'NONE', #7781 ) ;
#3722 = EDGE_CURVE ( 'NONE', #4474, #4547, #3749, .T. ) ;
#3723 =( NAMED_UNIT ( * ) SI_UNIT ( $, .STERADIAN. ) SOLID_ANGLE_UNIT ( ) );
#3724 = DIRECTION ( 'NONE',  ( -1.000000000000000000, -1.261617073437677999E-16, 0.000000000000000000 ) ) ;
#3725 = DIRECTION ( 'NONE',  ( 0.000000000000000000, 0.000000000000000000, 1.000000000000000000 ) ) ;
#3726 = EDGE_CURVE ( 'NONE', #3478, #2004, #641, .T. ) ;
#3727 = CARTESIAN_POINT ( 'NONE',  ( 0.000000000000000000, 0.000000000000000000, 0.000000000000000000 ) ) ;
#3728 = ORIENTED_EDGE ( 'NONE', *, *, #1649, .F. ) ;
#3729 = CARTESIAN_POINT ( 'NONE',  ( 398.0000000000001137, 12.50000000000000000, -15.61249499599599488 ) ) ;
#3730 = SHAPE_REPRESENTATION ( 'Handle', ( #5785 ), #5126 ) ;
#3731 = APPLICATION_CONTEXT ( 'automotive_design' ) ;
#3732 = EDGE_LOOP ( 'NONE', ( #3059, #1674, #5738, #4044 ) ) ;
#3733 = CARTESIAN_POINT ( 'NONE',  ( 362.8398061413552114, 19.78928940797825931, -2.924464941254242056 ) ) ;
#3734 = ORIENTED_EDGE ( 'NONE', *, *, #4427, .T. ) ;
#3735 = CARTESIAN_POINT ( 'NONE',  ( -17.99038105676657651, 1.734723475976807094E-15, 7.500000000000000000 ) ) ;
#3736 = VERTEX_POINT ( 'NONE', #601 ) ;
#3737 = DIRECTION ( 'NONE',  ( -0.000000000000000000, 0.000000000000000000, 1.000000000000000000 ) ) ;
#3738 = CARTESIAN_POINT ( 'NONE',  ( 400.0000000000000568, -25.00000000000000000, 25.00000000000000000 ) ) ;
#3739 = ADVANCED_FACE ( 'NONE', ( #673, #7337, #4841 ), #2711, .F. ) ;
#3740 = ORIENTED_EDGE ( 'NONE', *, *, #3236, .F. ) ;
#3741 = ORIENTED_EDGE ( 'NONE', *, *, #1834, .F. ) ;
#3742 = ORIENTED_EDGE ( 'NONE', *, *, #3843, .F. ) ;
#3743 = CARTESIAN_POINT ( 'NONE',  ( 384.8984063742112767, -18.48201531705921141, 7.676572043282099855 ) ) ;
#3744 = CARTESIAN_POINT ( 'NONE',  ( 387.3963605620842827, -19.93536271250352598, 1.660494579713906127 ) ) ;
#3745 = DIRECTION ( 'NONE',  ( -0.000000000000000000, -1.000000000000000000, -0.000000000000000000 ) ) ;
#3746 = LINE ( 'NONE', #4328, #2212 ) ;
#3747 = AXIS2_PLACEMENT_3D ( 'NONE', #5717, #214, #7556 ) ;
#3748 = DIRECTION ( 'NONE',  ( -1.000000000000000000, 1.224646799147353454E-16, 0.000000000000000000 ) ) ;
#3749 = B_SPLINE_CURVE_WITH_KNOTS ( 'NONE', 3,
 ( #2932, #2290, #1193, #4278, #1829, #1715, #1237, #7301, #4240, #29, #5530, #1798, #6690, #4160, #6054, #2478, #4878, #66, #3568, #3093, #7260, #7219, #6616, #4798, #5451, #6774, #2363, #5405, #6173, #1757, #1870, #4201, #4918, #6729, #6657, #3693, #1160, #3646, #3606, #560, #3128, #6017, #4317, #1279, #3009, #6132, #1116, #6095, #523, #2972, #7888, #5491, #7850, #7377 ),
 .UNSPECIFIED., .F., .F.,
 ( 4, 2, 2, 2, 2, 2, 2, 2, 2, 2, 2, 2, 2, 2, 2, 2, 2, 2, 2, 2, 2, 2, 2, 2, 2, 2, 4 ),
 ( 0.04018604478735846031, 0.04269101871805709714, 0.04394350568340633229, 0.04519599264875557437, 0.04644847961410480952, 0.04770096657945405161, 0.05020594051015265374, 0.05145842747550190277, 0.05271091444085115874, 0.05521588837154975393, 0.05646837533689905153, 0.05772086230224834913, 0.05897334926759764673, 0.06022583623294694433, 0.06273081016364553952, 0.06398329712899483712, 0.06523578409434413472, 0.06648827105969341844, 0.06774075802504271604, 0.07024573195574131124, 0.07149821892109066435, 0.07275070588644001746, 0.07525567981713872368, 0.07650816678248806291, 0.07776065374783742989, 0.07901314071318678300, 0.08026562767853613611 ),
 .UNSPECIFIED. ) ;
#3750 = DIRECTION ( 'NONE',  ( -1.000000000000000000, 0.000000000000000000, -0.000000000000000000 ) ) ;
#3751 = CARTESIAN_POINT ( 'NONE',  ( 340.0000000000000000, 0.000000000000000000, 0.000000000000000000 ) ) ;
#3752 = LINE ( 'NONE', #849, #2619 ) ;
#3753 = DIRECTION ( 'NONE',  ( 1.000000000000000000, 0.000000000000000000, 0.000000000000000000 ) ) ;
#3754 = EDGE_LOOP ( 'NONE', ( #3688, #3998, #353, #2892 ) ) ;
#3755 = EDGE_CURVE ( 'NONE', #3564, #7759, #2518, .T. ) ;
#3756 = ORIENTED_EDGE ( 'NONE', *, *, #2485, .T. ) ;
#3757 = DIRECTION ( 'NONE',  ( 0.000000000000000000, 0.000000000000000000, 1.000000000000000000 ) ) ;
#3758 = LINE ( 'NONE', #1339, #2148 ) ;
#3759 = CARTESIAN_POINT ( 'NONE',  ( 0.000000000000000000, 0.000000000000000000, 0.000000000000000000 ) ) ;
#3760 = EDGE_CURVE ( 'NONE', #2355, #3881, #3672, .T. ) ;
#3761 = LINE ( 'NONE', #177, #5566 ) ;
#3762 = EDGE_LOOP ( 'NONE', ( #2409, #6330, #3136, #1954, #3194, #2818, #1716, #3007, #7324, #6506, #7854, #6310, #3987, #1245, #285, #384, #6866, #3652, #4161, #5809, #7804, #3250, #4311, #6352, #1479, #4031 ) ) ;
#3763 = CARTESIAN_POINT ( 'NONE',  ( 75.00000000000000000, 10.56842436860067735, 25.00000000000000000 ) ) ;
#3764 = ADVANCED_FACE ( 'NONE', ( #3768 ), #845, .T. ) ;
#3765 = ADVANCED_FACE ( 'NONE', ( #1470 ), #7491, .F. ) ;
#3766 = DIRECTION ( 'NONE',  ( -1.000000000000000000, 0.000000000000000000, 0.000000000000000000 ) ) ;
#3767 = ORIENTED_EDGE ( 'NONE', *, *, #4293, .F. ) ;
#3768 = FACE_OUTER_BOUND ( 'NONE', #3313, .T. ) ;
#3769 = ORIENTED_EDGE ( 'NONE', *, *, #5870, .F. ) ;
#3770 = CARTESIAN_POINT ( 'NONE',  ( -6.495190528383286477, 16.25000000000000000, 0.000000000000000000 ) ) ;
#3771 = AXIS2_PLACEMENT_3D ( 'NONE', #4891, #1770, #7313 ) ;
#3772 = ORIENTED_EDGE ( 'NONE', *, *, #3718, .T. ) ;
#3773 = VERTEX_POINT ( 'NONE', #5729 ) ;
#3774 = ORIENTED_EDGE ( 'NONE', *, *, #1052, .T. ) ;
#3775 = DIRECTION ( 'NONE',  ( 1.224646799147353207E-16, 1.000000000000000000, -0.000000000000000000 ) ) ;
#3776 = DIRECTION ( 'NONE',  ( 1.000000000000000000, 0.000000000000000000, 0.000000000000000000 ) ) ;
#3777 = DIRECTION ( 'NONE',  ( 0.000000000000000000, -0.000000000000000000, -1.000000000000000000 ) ) ;
#3778 = DIRECTION ( 'NONE',  ( 0.000000000000000000, -0.000000000000000000, -1.000000000000000000 ) ) ;
#3779 = AXIS2_PLACEMENT_3D ( 'NONE', #383, #1502, #2273 ) ;
#3780 = CIRCLE ( 'NONE', #953, 12.50000000000001066 ) ;
#3781 = DIRECTION ( 'NONE',  ( -0.000000000000000000, 0.000000000000000000, 1.000000000000000000 ) ) ;
#3782 = CIRCLE ( 'NONE', #316, 74.99999999999995737 ) ;
#3783 = VECTOR ( 'NONE', #971, 1000.000000000000000 ) ;
#3784 = EDGE_CURVE ( 'NONE', #481, #3051, #6890, .T. ) ;
#3785 = ITEM_DEFINED_TRANSFORMATION ( 'NONE', 'NONE', #1934,  #5785 ) ;
#3786 = CARTESIAN_POINT ( 'NONE',  ( 2.775557561562891351E-14, 262.5000000000000568, 12.50000000000000000 ) ) ;
#3787 = DIRECTION ( 'NONE',  ( 0.000000000000000000, 0.000000000000000000, 1.000000000000000000 ) ) ;
#3788 = CARTESIAN_POINT ( 'NONE',  ( 38.21904415029484170, 19.40417101989674009, 12.50000000000000000 ) ) ;
#3789 = DIRECTION ( 'NONE',  ( 0.000000000000000000, 0.000000000000000000, -1.000000000000000000 ) ) ;
#3790 = VECTOR ( 'NONE', #7411, 1000.000000000000000 ) ;
#3791 = ORIENTED_EDGE ( 'NONE', *, *, #4262, .F. ) ;
#3792 = ORIENTED_EDGE ( 'NONE', *, *, #3565, .T. ) ;
#3793 = CARTESIAN_POINT ( 'NONE',  ( 0.000000000000000000, 0.000000000000000000, 6.999999999999999112 ) ) ;
#3794 = CARTESIAN_POINT ( 'NONE',  ( 412.5000000000002274, 1.221245327087672598E-12, 0.000000000000000000 ) ) ;
#3795 = FACE_OUTER_BOUND ( 'NONE', #5960, .T. ) ;
#3796 = DIRECTION ( 'NONE',  ( 1.000000000000000000, 0.000000000000000000, 0.000000000000000000 ) ) ;
#3797 = VERTEX_POINT ( 'NONE', #6212 ) ;
#3798 = DIRECTION ( 'NONE',  ( -0.000000000000000000, -0.000000000000000000, -1.000000000000000000 ) ) ;
#3799 = MECHANICAL_DESIGN_GEOMETRIC_PRESENTATION_REPRESENTATION (  '', ( #1358 ), #7773 ) ;
#3800 = ORIENTED_EDGE ( 'NONE', *, *, #5093, .F. ) ;
#3801 = CARTESIAN_POINT ( 'NONE',  ( 365.9011734668954432, 18.06872101906905215, -8.580138959277956445 ) ) ;
#3802 = VERTEX_POINT ( 'NONE', #6286 ) ;
#3803 = FACE_OUTER_BOUND ( 'NONE', #4210, .T. ) ;
#3804 = EDGE_LOOP ( 'NONE', ( #7338, #292, #6255, #794 ) ) ;
#3805 = DIRECTION ( 'NONE',  ( 0.000000000000000000, -1.000000000000000000, 0.000000000000000000 ) ) ;
#3806 = LINE ( 'NONE', #1241, #3395 ) ;
#3807 = EDGE_CURVE ( 'NONE', #3094, #3133, #6965, .T. ) ;
#3808 = CIRCLE ( 'NONE', #6241, 10.49999999999999467 ) ;
#3809 = EDGE_CURVE ( 'NONE', #1399, #2876, #7416, .T. ) ;
#3810 = VERTEX_POINT ( 'NONE', #1426 ) ;
#3811 = ORIENTED_EDGE ( 'NONE', *, *, #4990, .T. ) ;
#3812 = EDGE_LOOP ( 'NONE', ( #5393, #943, #485, #3846 ) ) ;
#3813 = CARTESIAN_POINT ( 'NONE',  ( -20.00000000000000000, 0.000000000000000000, 52.50000000000000000 ) ) ;
#3814 = LINE ( 'NONE', #6186, #1249 ) ;
#3815 = EDGE_CURVE ( 'NONE', #3493, #3094, #1610, .T. ) ;
#3816 = VERTEX_POINT ( 'NONE', #3917 ) ;
#3817 = FACE_OUTER_BOUND ( 'NONE', #6401, .T. ) ;
#3818 = CIRCLE ( 'NONE', #6639, 12.50000000000000355 ) ;
#3819 = DIRECTION ( 'NONE',  ( -0.000000000000000000, -0.000000000000000000, -1.000000000000000000 ) ) ;
#3820 = DIRECTION ( 'NONE',  ( -0.000000000000000000, -0.000000000000000000, -1.000000000000000000 ) ) ;
#3821 = DIRECTION ( 'NONE',  ( 0.000000000000000000, 0.000000000000000000, -1.000000000000000000 ) ) ;
#3822 = DIRECTION ( 'NONE',  ( -1.000000000000000000, -0.000000000000000000, -0.000000000000000000 ) ) ;
#3823 = AXIS2_PLACEMENT_3D ( 'NONE', #1472, #304, #435 ) ;
#3824 = AXIS2_PLACEMENT_3D ( 'NONE', #5994, #1967, #6115 ) ;
#3825 = EDGE_CURVE ( 'NONE', #4302, #1554, #1478, .T. ) ;
#3826 = EDGE_LOOP ( 'NONE', ( #2188, #4142 ) ) ;
#3827 = CARTESIAN_POINT ( 'NONE',  ( 398.0000000000001137, -12.50000000000000000, -15.61249499599599488 ) ) ;
#3828 = CIRCLE ( 'NONE', #5228, 0.5000000000000004441 ) ;
#3829 = AXIS2_PLACEMENT_3D ( 'NONE', #2862, #4009, #6464 ) ;
#3830 = ORIENTED_EDGE ( 'NONE', *, *, #7440, .F. ) ;
#3831 = DIRECTION ( 'NONE',  ( 0.000000000000000000, 0.000000000000000000, -1.000000000000000000 ) ) ;
#3832 = CARTESIAN_POINT ( 'NONE',  ( -27.49999999999989342, 182.4999999999999432, 0.000000000000000000 ) ) ;
#3833 = DIRECTION ( 'NONE',  ( 1.000000000000000000, 0.000000000000000000, 0.000000000000000000 ) ) ;
#3834 = CARTESIAN_POINT ( 'NONE',  ( 375.0000000000000000, 12.50000000000000000, 12.50000000000000711 ) ) ;
#3835 = VERTEX_POINT ( 'NONE', #1314 ) ;
#3836 = LINE ( 'NONE', #3468, #3028 ) ;
#3837 = VECTOR ( 'NONE', #1510, 1000.000000000000000 ) ;
#3838 = UNCERTAINTY_MEASURE_WITH_UNIT (LENGTH_MEASURE( 1.000000000000000082E-05 ), #2584, 'distance_accuracy_value', 'NONE');
#3839 = CARTESIAN_POINT ( 'NONE',  ( 365.1015936257888939, 18.48201531705921141, 7.676572043282099855 ) ) ;
#3840 = ORIENTED_EDGE ( 'NONE', *, *, #3629, .T. ) ;
#3841 = CARTESIAN_POINT ( 'NONE',  ( 12.50000000000000000, 1.530808498934191521E-15, 2.000000000000001776 ) ) ;
#3842 = VERTEX_POINT ( 'NONE', #110 ) ;
#3843 = EDGE_CURVE ( 'NONE', #5237, #243, #4389, .T. ) ;
#3844 = DIRECTION ( 'NONE',  ( -1.000000000000000000, -0.000000000000000000, -0.000000000000000000 ) ) ;
#3845 = CARTESIAN_POINT ( 'NONE',  ( -25.00000000000000000, 1.530808498934191521E-15, 12.50000000000000000 ) ) ;
#3846 = ORIENTED_EDGE ( 'NONE', *, *, #3675, .F. ) ;
#3847 = LINE ( 'NONE', #5082, #3712 ) ;
#3848 = ORIENTED_EDGE ( 'NONE', *, *, #6502, .T. ) ;
#3849 = ADVANCED_FACE ( 'NONE', ( #3803 ), #750, .F. ) ;
#3850 = VERTEX_POINT ( 'NONE', #788 ) ;
#3851 = CARTESIAN_POINT ( 'NONE',  ( 0.000000000000000000, 0.000000000000000000, 0.000000000000000000 ) ) ;
#3852 = DIRECTION ( 'NONE',  ( 0.000000000000000000, 0.000000000000000000, 1.000000000000000000 ) ) ;
#3853 = CARTESIAN_POINT ( 'NONE',  ( 200.0000000000000000, -37.50000000000000711, 0.000000000000000000 ) ) ;
#3854 = ORIENTED_EDGE ( 'NONE', *, *, #5719, .T. ) ;
#3855 = EDGE_CURVE ( 'NONE', #5478, #279, #3206, .T. ) ;
#3856 = CARTESIAN_POINT ( 'NONE',  ( 12.50000000000000000, -24.99999999999999645, -3.235013004037443297E-15 ) ) ;
#3857 = ADVANCED_FACE ( 'NONE', ( #3877 ), #5074, .F. ) ;
#3858 = PRODUCT ( 'Connector', 'Connector', '', ( #1927 ) ) ;
#3859 = ITEM_DEFINED_TRANSFORMATION ( 'NONE', 'NONE', #3612,  #5785 ) ;
#3860 = CARTESIAN_POINT ( 'NONE',  ( 375.0000000000000000, -15.61249499599599488, -12.50000000000000000 ) ) ;
#3861 = FACE_OUTER_BOUND ( 'NONE', #4688, .T. ) ;
#3862 = CARTESIAN_POINT ( 'NONE',  ( 46.25000000000002842, 111.9999999999999005, 130.0000000000000000 ) ) ;
#3863 = CARTESIAN_POINT ( 'NONE',  ( -32.49999999999990052, 177.4999999999999432, 5.000000000000000000 ) ) ;
#3864 = VERTEX_POINT ( 'NONE', #3841 ) ;
#3865 = CARTESIAN_POINT ( 'NONE',  ( 400.0000000000000000, -12.50000000000000000, -12.95183384698871798 ) ) ;
#3866 = DIRECTION ( 'NONE',  ( 0.8884260488187299964, -4.255279772943761115E-16, 0.4590197771124243098 ) ) ;
#3867 = ORIENTED_EDGE ( 'NONE', *, *, #3537, .F. ) ;
#3868 =( NAMED_UNIT ( * ) SI_UNIT ( $, .STERADIAN. ) SOLID_ANGLE_UNIT ( ) );
#3869 = DIRECTION ( 'NONE',  ( 1.000000000000000000, 0.000000000000000000, 0.000000000000000000 ) ) ;
#3870 = DIRECTION ( 'NONE',  ( 0.000000000000000000, 0.000000000000000000, 1.000000000000000000 ) ) ;
#3871 = DIRECTION ( 'NONE',  ( 1.000000000000000000, 0.000000000000000000, 0.000000000000000000 ) ) ;
#3872 = ORIENTED_EDGE ( 'NONE', *, *, #4966, .T. ) ;
#3873 = EDGE_LOOP ( 'NONE', ( #5847, #5882, #3373, #3962 ) ) ;
#3874 = CARTESIAN_POINT ( 'NONE',  ( 46.25000000000002842, 47.50000000000003553, 17.50000000000000000 ) ) ;
#3875 = VERTEX_POINT ( 'NONE', #3239 ) ;
#3876 = EDGE_CURVE ( 'NONE', #279, #846, #6323, .T. ) ;
#3877 = FACE_OUTER_BOUND ( 'NONE', #399, .T. ) ;
#3878 = EDGE_LOOP ( 'NONE', ( #5073, #4018, #6779, #5652 ) ) ;
#3879 = DIRECTION ( 'NONE',  ( -1.000000000000000000, 0.000000000000000000, 0.000000000000000000 ) ) ;
#3880 = DIRECTION ( 'NONE',  ( 0.000000000000000000, 0.000000000000000000, 1.000000000000000000 ) ) ;
#3881 = VERTEX_POINT ( 'NONE', #5113 ) ;
#3882 = DIRECTION ( 'NONE',  ( 1.000000000000000000, 0.000000000000000000, 0.000000000000000000 ) ) ;
#3883 = ORIENTED_EDGE ( 'NONE', *, *, #7596, .F. ) ;
#3884 = ORIENTED_EDGE ( 'NONE', *, *, #1065, .F. ) ;
#3885 = DIRECTION ( 'NONE',  ( 1.000000000000000000, -3.469446951953614189E-17, 0.000000000000000000 ) ) ;
#3886 = CARTESIAN_POINT ( 'NONE',  ( 50.71904415029504065, 62.70544120911855401, 0.000000000000000000 ) ) ;
#3887 = CARTESIAN_POINT ( 'NONE',  ( 12.50000000000000000, 1.530808498934191521E-15, 7.500000000000000000 ) ) ;
#3888 = EDGE_LOOP ( 'NONE', ( #1616, #1033 ) ) ;
#3889 = CARTESIAN_POINT ( 'NONE',  ( 25.00000000000000000, 0.000000000000000000, 0.000000000000000000 ) ) ;
#3890 = CIRCLE ( 'NONE', #1963, 0.5000000000000004441 ) ;
#3891 = AXIS2_PLACEMENT_3D ( 'NONE', #5679, #5519, #4266 ) ;
#3892 = EDGE_CURVE ( 'NONE', #7913, #957, #5588, .T. ) ;
#3893 = AXIS2_PLACEMENT_3D ( 'NONE', #2501, #1332, #584 ) ;
#3894 = DIRECTION ( 'NONE',  ( 1.000000000000000000, -0.000000000000000000, -0.000000000000000000 ) ) ;
#3895 = DIRECTION ( 'NONE',  ( 1.000000000000000000, 0.000000000000000000, 0.000000000000000000 ) ) ;
#3896 = DIRECTION ( 'NONE',  ( -1.000000000000000000, 0.000000000000000000, 0.000000000000000000 ) ) ;
#3897 = DIRECTION ( 'NONE',  ( 1.000000000000000000, 0.000000000000000000, -0.000000000000000000 ) ) ;
#3898 = ADVANCED_FACE ( 'NONE', ( #5770, #269 ), #2192, .F. ) ;
#3899 = EDGE_CURVE ( 'NONE', #7081, #5007, #6611, .T. ) ;
#3900 = AXIS2_PLACEMENT_3D ( 'NONE', #5773, #4516, #1473 ) ;
#3901 = CIRCLE ( 'NONE', #6086, 5.000000000000000000 ) ;
#3902 = ORIENTED_EDGE ( 'NONE', *, *, #1831, .F. ) ;
#3903 = EDGE_CURVE ( 'NONE', #3018, #2853, #906, .T. ) ;
#3904 = CARTESIAN_POINT ( 'NONE',  ( 0.000000000000000000, 0.000000000000000000, -18.75000000000009948 ) ) ;
#3905 = ORIENTED_EDGE ( 'NONE', *, *, #7525, .F. ) ;
#3906 = LINE ( 'NONE', #3474, #4176 ) ;
#3907 = LINE ( 'NONE', #7075, #5616 ) ;
#3909 = DIRECTION ( 'NONE',  ( -0.000000000000000000, -0.000000000000000000, -1.000000000000000000 ) ) ;
#3908 = VECTOR ( 'NONE', #4673, 1000.000000000000000 ) ;
#3910 = LINE ( 'NONE', #6281, #3141 ) ;
#3911 = EDGE_LOOP ( 'NONE', ( #7105, #7874 ) ) ;
#3912 = ADVANCED_FACE ( 'NONE', ( #6532 ), #2280, .F. ) ;
#3913 = ADVANCED_FACE ( 'NONE', ( #7724 ), #7085, .T. ) ;
#3914 = ORIENTED_EDGE ( 'NONE', *, *, #7296, .T. ) ;
#3915 = CARTESIAN_POINT ( 'NONE',  ( 0.7190441502950353225, 62.70544120911855401, 0.000000000000000000 ) ) ;
#3916 = EDGE_LOOP ( 'NONE', ( #4595, #6602, #1650, #3559, #2933, #4285, #3983, #5484 ) ) ;
#3917 = CARTESIAN_POINT ( 'NONE',  ( -27.49999999999994671, 37.50000000000008527, 0.000000000000000000 ) ) ;
#3918 = ORIENTED_EDGE ( 'NONE', *, *, #6756, .T. ) ;
#3919 = DIRECTION ( 'NONE',  ( -1.000000000000000000, 4.270088556250607616E-16, -0.000000000000000000 ) ) ;
#3920 = CARTESIAN_POINT ( 'NONE',  ( 11.64999999999996660, 1.671642880836134930E-15, 200.0000000000000000 ) ) ;
#3921 = EDGE_CURVE ( 'NONE', #7220, #5242, #973, .T. ) ;
#3922 = VERTEX_POINT ( 'NONE', #7007 ) ;
#3923 = CIRCLE ( 'NONE', #1614, 15.00000000000000000 ) ;
#3924 = DIRECTION ( 'NONE',  ( -0.000000000000000000, -0.000000000000000000, -1.000000000000000000 ) ) ;
#3925 = ORIENTED_EDGE ( 'NONE', *, *, #7553, .T. ) ;
#3926 = ORIENTED_EDGE ( 'NONE', *, *, #5670, .T. ) ;
#3927 = APPLICATION_CONTEXT ( 'automotive_design' ) ;
#3928 = ADVANCED_BREP_SHAPE_REPRESENTATION ( '', ( #1383, #5785 ), #4108 ) ;
#3929 = CARTESIAN_POINT ( 'NONE',  ( 325.0000000000000000, -12.50000000000000000, 25.00000000000000000 ) ) ;
#3930 = CARTESIAN_POINT ( 'NONE',  ( -25.00000000000000000, 0.000000000000000000, 0.000000000000000000 ) ) ;
#3931 = DIRECTION ( 'NONE',  ( 1.000000000000000000, 0.000000000000000000, 0.000000000000000000 ) ) ;
#3932 = AXIS2_PLACEMENT_3D ( 'NONE', #3625, #4221, #2991 ) ;
#3933 = ORIENTED_EDGE ( 'NONE', *, *, #276, .F. ) ;
#3934 = AXIS2_PLACEMENT_3D ( 'NONE', #3022, #5339, #7310 ) ;
#3935 = CARTESIAN_POINT ( 'NONE',  ( 353.4483633286965301, 150.0000000000000284, 138.3903618369216417 ) ) ;
#3936 = LINE ( 'NONE', #5789, #5102 ) ;
#3937 = DIRECTION ( 'NONE',  ( 1.000000000000000000, 0.000000000000000000, 0.000000000000000000 ) ) ;
#3938 = DIRECTION ( 'NONE',  ( 0.000000000000000000, -1.000000000000000000, -0.000000000000000000 ) ) ;
#3939 = MECHANICAL_DESIGN_GEOMETRIC_PRESENTATION_REPRESENTATION (  '', ( #6768 ), #5239 ) ;
#3940 = VECTOR ( 'NONE', #1402, 1000.000000000000000 ) ;
#3941 = EDGE_LOOP ( 'NONE', ( #6883, #1990 ) ) ;
#3942 = CARTESIAN_POINT ( 'NONE',  ( 589.6646527764517032, 177.1990734970207768, 551.8904258943550758 ) ) ;
#3943 = ORIENTED_EDGE ( 'NONE', *, *, #4882, .T. ) ;
#3944 = AXIS2_PLACEMENT_3D ( 'NONE', #5347, #5991, #2785 ) ;
#3945 = ADVANCED_FACE ( 'NONE', ( #4709 ), #2236, .F. ) ;
#3946 = CARTESIAN_POINT ( 'NONE',  ( 199.9999999999998863, 225.0000000000000284, 12.50000000000000000 ) ) ;
#3947 = CARTESIAN_POINT ( 'NONE',  ( 2.775557561562891351E-14, 225.0000000000000284, 0.000000000000000000 ) ) ;
#3948 = VECTOR ( 'NONE', #5180, 1000.000000000000000 ) ;
#3949 = CARTESIAN_POINT ( 'NONE',  ( -6.495190528383282036, -16.24999999999999645, 7.500000000000000000 ) ) ;
#3950 = CARTESIAN_POINT ( 'NONE',  ( 2.775557561562891351E-14, 225.0000000000000284, 12.50000000000000000 ) ) ;
#3951 = ORIENTED_EDGE ( 'NONE', *, *, #323, .T. ) ;
#3952 = ADVANCED_FACE ( 'NONE', ( #2759 ), #7175, .T. ) ;
#3953 = AXIS2_PLACEMENT_3D ( 'NONE', #3030, #4480, #6034 ) ;
#3954 = CARTESIAN_POINT ( 'NONE',  ( -8.959197987552832032, 23.33951095074251114, 0.000000000000000000 ) ) ;
#3955 = ORIENTED_EDGE ( 'NONE', *, *, #5862, .F. ) ;
#3956 = DIRECTION ( 'NONE',  ( -0.000000000000000000, 0.000000000000000000, 1.000000000000000000 ) ) ;
#3957 = CARTESIAN_POINT ( 'NONE',  ( 2.775557561562891351E-14, 262.5000000000000568, 0.000000000000000000 ) ) ;
#3958 = VECTOR ( 'NONE', #1712, 1000.000000000000000 ) ;
#3959 = CARTESIAN_POINT ( 'NONE',  ( 296.6025403784437913, 0.000000000000000000, 12.50000000000000000 ) ) ;
#3960 = CIRCLE ( 'NONE', #5758, 17.50000000000000355 ) ;
#3961 = CARTESIAN_POINT ( 'NONE',  ( 200.0000000000000000, 0.000000000000000000, 0.000000000000000000 ) ) ;
#3962 = ORIENTED_EDGE ( 'NONE', *, *, #7765, .T. ) ;
#3963 = CARTESIAN_POINT ( 'NONE',  ( -25.00000000000000000, 0.000000000000000000, -12.50000000000000000 ) ) ;
#3964 = ORIENTED_EDGE ( 'NONE', *, *, #7639, .F. ) ;
#3965 = DIRECTION ( 'NONE',  ( 0.000000000000000000, 0.000000000000000000, 1.000000000000000000 ) ) ;
#3966 = EDGE_LOOP ( 'NONE', ( #7520, #2471, #6573, #7425 ) ) ;
#3967 = DIRECTION ( 'NONE',  ( 0.000000000000000000, 0.000000000000000000, 1.000000000000000000 ) ) ;
#3968 = ADVANCED_FACE ( 'NONE', ( #432 ), #7049, .F. ) ;
#3969 = CARTESIAN_POINT ( 'NONE',  ( -37.50000000000000000, 4.592427351555481498E-15, 12.50000000000000000 ) ) ;
#3970 = DIRECTION ( 'NONE',  ( -1.000000000000000000, 1.094506615593124476E-16, 0.000000000000000000 ) ) ;
#3971 = CARTESIAN_POINT ( 'NONE',  ( -48.67326389759909944, 48.65950482248330644, 0.000000000000000000 ) ) ;
#3972 = ORIENTED_EDGE ( 'NONE', *, *, #1263, .F. ) ;
#3973 = DIRECTION ( 'NONE',  ( 0.000000000000000000, 0.000000000000000000, -1.000000000000000000 ) ) ;
#3974 = DIRECTION ( 'NONE',  ( 1.000000000000000000, 0.000000000000000000, 0.000000000000000000 ) ) ;
#3975 = DIRECTION ( 'NONE',  ( -1.000000000000000000, 0.000000000000000000, 0.000000000000000000 ) ) ;
#3976 = FACE_OUTER_BOUND ( 'NONE', #1958, .T. ) ;
#3977 = CARTESIAN_POINT ( 'NONE',  ( 50.71904415029504065, 62.70544120911855401, 12.50000000000000000 ) ) ;
#3978 = DIRECTION ( 'NONE',  ( 9.051261995106130006E-33, -0.9242245927363030855, -0.3818493186865927203 ) ) ;
#3979 = EDGE_LOOP ( 'NONE', ( #4027, #1145, #662, #5840 ) ) ;
#3980 = FILL_AREA_STYLE ('',( #4063 ) ) ;
#3981 = CARTESIAN_POINT ( 'NONE',  ( 400.0000000000000568, 25.00000000000000000, 25.00000000000000000 ) ) ;
#3982 = LINE ( 'NONE', #1500, #3008 ) ;
#3983 = ORIENTED_EDGE ( 'NONE', *, *, #4811, .T. ) ;
#3984 = CARTESIAN_POINT ( 'NONE',  ( 0.000000000000000000, 113.0000000000000426, 130.0000000000000000 ) ) ;
#3985 = PRODUCT_DEFINITION_CONTEXT ( 'detailed design', #7820, 'design' ) ;
#3986 = EDGE_CURVE ( 'NONE', #52, #6264, #7261, .T. ) ;
#3987 = ORIENTED_EDGE ( 'NONE', *, *, #2213, .T. ) ;
#3988 = EDGE_CURVE ( 'NONE', #511, #7515, #6407, .T. ) ;
#3989 = DIRECTION ( 'NONE',  ( -0.000000000000000000, 0.000000000000000000, -1.000000000000000000 ) ) ;
#3990 = VERTEX_POINT ( 'NONE', #2879 ) ;
#3991 = DIRECTION ( 'NONE',  ( -0.000000000000000000, 0.000000000000000000, 1.000000000000000000 ) ) ;
#3992 = ORIENTED_EDGE ( 'NONE', *, *, #7639, .T. ) ;
#3993 = CYLINDRICAL_SURFACE ( 'NONE', #7914, 5.000000000000004441 ) ;
#3994 = FACE_OUTER_BOUND ( 'NONE', #6246, .T. ) ;
#3995 = EDGE_CURVE ( 'NONE', #4376, #5884, #5276, .T. ) ;
#3996 = AXIS2_PLACEMENT_3D ( 'NONE', #5943, #6627, #6030 ) ;
#3997 = EDGE_CURVE ( 'NONE', #7839, #7303, #3923, .T. ) ;
#3998 = ORIENTED_EDGE ( 'NONE', *, *, #7243, .T. ) ;
#3999 = CARTESIAN_POINT ( 'NONE',  ( 339.1025403784438481, 142.5000000000000000, 125.0000000000000000 ) ) ;
#4000 = ORIENTED_EDGE ( 'NONE', *, *, #6041, .F. ) ;
#4001 = CARTESIAN_POINT ( 'NONE',  ( 296.6025403784437913, 142.5000000000000000, 155.0000000000000000 ) ) ;
#4002 = EDGE_LOOP ( 'NONE', ( #4795, #3972, #2688, #6659, #759, #6643, #120 ) ) ;
#4003 = DIRECTION ( 'NONE',  ( 0.000000000000000000, 0.000000000000000000, -1.000000000000000000 ) ) ;
#4004 = DIRECTION ( 'NONE',  ( 0.000000000000000000, 0.000000000000000000, 1.000000000000000000 ) ) ;
#4005 = CARTESIAN_POINT ( 'NONE',  ( 162.5000000000000000, 1.990051048614448997E-14, 25.00000000000000000 ) ) ;
#4006 = CARTESIAN_POINT ( 'NONE',  ( 325.0000000000000000, 0.000000000000000000, 25.00000000000000000 ) ) ;
#4007 = ORIENTED_EDGE ( 'NONE', *, *, #3327, .F. ) ;
#4008 = CARTESIAN_POINT ( 'NONE',  ( 0.000000000000000000, 87.70544117646394966, 12.50000000000000000 ) ) ;
#4009 = DIRECTION ( 'NONE',  ( -0.000000000000000000, -0.000000000000000000, -1.000000000000000000 ) ) ;
#4010 = DIRECTION ( 'NONE',  ( 0.000000000000000000, 0.000000000000000000, 1.000000000000000000 ) ) ;
#4011 = CIRCLE ( 'NONE', #5574, 12.50000000000000000 ) ;
#4012 = CARTESIAN_POINT ( 'NONE',  ( 175.0000000000000000, 1.836970198721029589E-15, -15.00000000000000000 ) ) ;
#4013 = CARTESIAN_POINT ( 'NONE',  ( 200.0000000000000000, 0.000000000000000000, 12.50000000000000000 ) ) ;
#4014 = EDGE_CURVE ( 'NONE', #4926, #1637, #2391, .T. ) ;
#4015 = AXIS2_PLACEMENT_3D ( 'NONE', #3759, #5554, #7408 ) ;
#4016 = CYLINDRICAL_SURFACE ( 'NONE', #6266, 31.24999999999999289 ) ;
#4017 = CARTESIAN_POINT ( 'NONE',  ( 332.3707862481380744, 194.6990734970208052, 245.6227876318357914 ) ) ;
#4018 = ORIENTED_EDGE ( 'NONE', *, *, #5620, .F. ) ;
#4019 = DIRECTION ( 'NONE',  ( 0.9335804380297001437, 0.3583679195021130526, 0.000000000000000000 ) ) ;
#4020 = DIRECTION ( 'NONE',  ( 0.000000000000000000, 0.000000000000000000, -1.000000000000000000 ) ) ;
#4021 = CARTESIAN_POINT ( 'NONE',  ( -37.49999999999994316, 225.0000000000000284, 12.50000000000000000 ) ) ;
#4022 = DIRECTION ( 'NONE',  ( 0.000000000000000000, 0.000000000000000000, 1.000000000000000000 ) ) ;
#4023 = ORIENTED_EDGE ( 'NONE', *, *, #7884, .T. ) ;
#4024 = CIRCLE ( 'NONE', #2244, 37.50000000000000711 ) ;
#4025 = ORIENTED_EDGE ( 'NONE', *, *, #4924, .T. ) ;
#4026 =( REPRESENTATION_RELATIONSHIP ('NONE','NONE', #6292, #6180 ) REPRESENTATION_RELATIONSHIP_WITH_TRANSFORMATION ( #2461 )SHAPE_REPRESENTATION_RELATIONSHIP( ) );
#4027 = ORIENTED_EDGE ( 'NONE', *, *, #1491, .T. ) ;
#4028 = AXIS2_PLACEMENT_3D ( 'NONE', #3961, #6327, #2154 ) ;
#4029 = DIRECTION ( 'NONE',  ( 0.000000000000000000, 0.000000000000000000, 1.000000000000000000 ) ) ;
#4030 = VECTOR ( 'NONE', #4261, 1000.000000000000000 ) ;
#4031 = ORIENTED_EDGE ( 'NONE', *, *, #7893, .F. ) ;
#4032 = CARTESIAN_POINT ( 'NONE',  ( 0.7190441502950353225, 62.70544120911855401, 12.50000000000000000 ) ) ;
#4033 = ORIENTED_EDGE ( 'NONE', *, *, #4550, .T. ) ;
#4034 = MANIFOLD_SOLID_BREP ( 'Yükseklik-Ekstrüzyon1', #7600 ) ;
#4035 = PRODUCT_RELATED_PRODUCT_CATEGORY ( 'part', '', ( #7704 ) ) ;
#4036 = VERTEX_POINT ( 'NONE', #4148 ) ;
#4037 = FACE_OUTER_BOUND ( 'NONE', #3888, .T. ) ;
#4038 = CARTESIAN_POINT ( 'NONE',  ( 212.5000000000000284, 1.530808498934191916E-15, 12.50000000000000000 ) ) ;
#4039 = VERTEX_POINT ( 'NONE', #4829 ) ;
#4040 = DIRECTION ( 'NONE',  ( 0.000000000000000000, 0.000000000000000000, 1.000000000000000000 ) ) ;
#4041 = ORIENTED_EDGE ( 'NONE', *, *, #1863, .T. ) ;
#4042 = DIRECTION ( 'NONE',  ( -4.789677997474686366E-16, -1.000000000000000000, -0.000000000000000000 ) ) ;
#4043 = AXIS2_PLACEMENT_3D ( 'NONE', #4084, #3492, #7651 ) ;
#4044 = ORIENTED_EDGE ( 'NONE', *, *, #5227, .F. ) ;
#4045 = CARTESIAN_POINT ( 'NONE',  ( 400.0000000000000568, 0.000000000000000000, 25.00000000000000000 ) ) ;
#4046 = EDGE_CURVE ( 'NONE', #5244, #2838, #471, .T. ) ;
#4047 = DIRECTION ( 'NONE',  ( -0.000000000000000000, -0.000000000000000000, -1.000000000000000000 ) ) ;
#4048 = CARTESIAN_POINT ( 'NONE',  ( -12.50000000000000000, 24.99999999999999645, 37.50000000000000711 ) ) ;
#4049 = DIRECTION ( 'NONE',  ( -1.000000000000000000, 0.000000000000000000, 0.000000000000000000 ) ) ;
#4050 = EDGE_CURVE ( 'NONE', #7362, #6044, #4228, .T. ) ;
#4051 = MECHANICAL_DESIGN_GEOMETRIC_PRESENTATION_REPRESENTATION (  '', ( #7383 ), #5592 ) ;
#4052 = ORIENTED_EDGE ( 'NONE', *, *, #72, .F. ) ;
#4053 = EDGE_CURVE ( 'NONE', #7523, #4616, #630, .T. ) ;
#4054 = CARTESIAN_POINT ( 'NONE',  ( 0.000000000000000000, -37.50000000000000000, 12.50000000000000000 ) ) ;
#4055 = CARTESIAN_POINT ( 'NONE',  ( -37.49999999999989342, 177.4999999999999432, 5.000000000000000000 ) ) ;
#4057 = DIRECTION ( 'NONE',  ( 0.000000000000000000, -8.474984920802721991E-16, 1.000000000000000000 ) ) ;
#4056=STYLED_ITEM('',(#7969),#4352);
#4058 = DIRECTION ( 'NONE',  ( 1.000000000000000000, 0.000000000000000000, 0.000000000000000000 ) ) ;
#4059 = CARTESIAN_POINT ( 'NONE',  ( -12.50000000000000000, 0.000000000000000000, 25.00000000000000000 ) ) ;
#4060 = VECTOR ( 'NONE', #3776, 1000.000000000000000 ) ;
#4061 = DIRECTION ( 'NONE',  ( -0.000000000000000000, -0.000000000000000000, -1.000000000000000000 ) ) ;
#4062 = ORIENTED_EDGE ( 'NONE', *, *, #6944, .F. ) ;
#4063 = FILL_AREA_STYLE_COLOUR ( '', #6877 ) ;
#4064 = CARTESIAN_POINT ( 'NONE',  ( -61.78095584970497356, 12.70544120911856112, 0.000000000000000000 ) ) ;
#4065 = DIRECTION ( 'NONE',  ( -0.000000000000000000, -0.000000000000000000, -1.000000000000000000 ) ) ;
#4066 = EDGE_CURVE ( 'NONE', #4514, #5786, #1238, .T. ) ;
#4067 = EDGE_LOOP ( 'NONE', ( #197, #1946, #6181, #1484 ) ) ;
#4068 = PRODUCT_DEFINITION_CONTEXT ( 'detailed design', #3927, 'design' ) ;
#4069 = EDGE_LOOP ( 'NONE', ( #2805, #3848, #2837, #2603, #2912 ) ) ;
#4070 = ORIENTED_EDGE ( 'NONE', *, *, #6158, .F. ) ;
#4071 = CIRCLE ( 'NONE', #622, 5.000000000000000888 ) ;
#4072 = AXIS2_PLACEMENT_3D ( 'NONE', #1574, #4020, #2667 ) ;
#4073 = ORIENTED_EDGE ( 'NONE', *, *, #5147, .T. ) ;
#4074 = DIRECTION ( 'NONE',  ( 0.000000000000000000, 0.000000000000000000, 1.000000000000000000 ) ) ;
#4075 = DIRECTION ( 'NONE',  ( 1.000000000000000000, 0.000000000000000000, 0.000000000000000000 ) ) ;
#4076 = VERTEX_POINT ( 'NONE', #1148 ) ;
#4077 = DIRECTION ( 'NONE',  ( -0.000000000000000000, -0.000000000000000000, -1.000000000000000000 ) ) ;
#4078 = DIRECTION ( 'NONE',  ( 1.000000000000000000, 0.000000000000000000, 0.000000000000000000 ) ) ;
#4079 = AXIS2_PLACEMENT_3D ( 'NONE', #1537, #6953, #6311 ) ;
#4080 = ORIENTED_EDGE ( 'NONE', *, *, #5584, .F. ) ;
#4081 = CARTESIAN_POINT ( 'NONE',  ( 0.7190441502950353225, 62.70544120911855401, 12.50000000000000000 ) ) ;
#4082 = ORIENTED_EDGE ( 'NONE', *, *, #6640, .F. ) ;
#4083 = VECTOR ( 'NONE', #954, 1000.000000000000000 ) ;
#4084 = CARTESIAN_POINT ( 'NONE',  ( 0.000000000000000000, 0.000000000000000000, 0.000000000000000000 ) ) ;
#4085 = AXIS2_PLACEMENT_3D ( 'NONE', #769, #287, #1487 ) ;
#4086 = ORIENTED_EDGE ( 'NONE', *, *, #4386, .T. ) ;
#4087 = CARTESIAN_POINT ( 'NONE',  ( -49.28095584970496645, -62.29455879088143888, 12.50000000000000000 ) ) ;
#4088 = CARTESIAN_POINT ( 'NONE',  ( 52.50000000000000711, 47.50000000000003553, 12.50000000000000000 ) ) ;
#4089 = ORIENTED_EDGE ( 'NONE', *, *, #6858, .F. ) ;
#4090 = EDGE_CURVE ( 'NONE', #6561, #982, #1997, .T. ) ;
#4091 = ORIENTED_EDGE ( 'NONE', *, *, #4491, .T. ) ;
#4092 = EDGE_CURVE ( 'NONE', #642, #7501, #3542, .T. ) ;
#4093 = FACE_BOUND ( 'NONE', #4562, .T. ) ;
#4094 = FACE_OUTER_BOUND ( 'NONE', #548, .T. ) ;
#4095 = CARTESIAN_POINT ( 'NONE',  ( 47.50000000000000711, 47.50000000000003553, 0.000000000000000000 ) ) ;
#4096 = CARTESIAN_POINT ( 'NONE',  ( 400.0000000000000000, 12.50000000000000000, 25.00000000000000000 ) ) ;
#4097 = CARTESIAN_POINT ( 'NONE',  ( 340.0000000000000000, -12.50000000000000355, 15.61249499599599311 ) ) ;
#4098 = ADVANCED_FACE ( 'NONE', ( #4188 ), #7810, .F. ) ;
#4099 = CARTESIAN_POINT ( 'NONE',  ( 20.00000000000000000, 2.449293598294706513E-15, 45.00000000000000000 ) ) ;
#4100 = APPLICATION_PROTOCOL_DEFINITION ( 'draft international standard', 'automotive_design', 1998, #4893 ) ;
#4101 = ORIENTED_EDGE ( 'NONE', *, *, #7671, .T. ) ;
#4102 = CARTESIAN_POINT ( 'NONE',  ( 387.5000000000000568, 0.000000000000000000, 25.00000000000000000 ) ) ;
#4103 = CARTESIAN_POINT ( 'NONE',  ( 0.000000000000000000, 0.000000000000000000, 25.00000000000000000 ) ) ;
#4104 = CARTESIAN_POINT ( 'NONE',  ( -25.00000000000000000, 0.000000000000000000, 0.000000000000000000 ) ) ;
#4105 = CYLINDRICAL_SURFACE ( 'NONE', #1212, 12.50000000000000000 ) ;
#4106 = ORIENTED_EDGE ( 'NONE', *, *, #4134, .F. ) ;
#4107 = EDGE_CURVE ( 'NONE', #5527, #5402, #19, .T. ) ;
#4108 =( GEOMETRIC_REPRESENTATION_CONTEXT ( 3 ) GLOBAL_UNCERTAINTY_ASSIGNED_CONTEXT ( ( #783 ) ) GLOBAL_UNIT_ASSIGNED_CONTEXT ( ( #590, #1301, #5477 ) ) REPRESENTATION_CONTEXT ( 'NONE', 'WORKASPACE' ) );
#4109 = ORIENTED_EDGE ( 'NONE', *, *, #724, .F. ) ;
#4110 = CARTESIAN_POINT ( 'NONE',  ( 0.000000000000000000, 0.000000000000000000, 0.000000000000000000 ) ) ;
#4111 = ORIENTED_EDGE ( 'NONE', *, *, #4236, .T. ) ;
#4112 = SURFACE_STYLE_USAGE ( .BOTH. , #1672 ) ;
#4113 = DIRECTION ( 'NONE',  ( 1.000000000000000000, 0.000000000000000000, 0.000000000000000000 ) ) ;
#4114 = PRODUCT_DEFINITION_FORMATION_WITH_SPECIFIED_SOURCE ( 'ANY', '', #2776, .NOT_KNOWN. ) ;
#4115 = VERTEX_POINT ( 'NONE', #4264 ) ;
#4116 = SURFACE_STYLE_USAGE ( .BOTH. , #1675 ) ;
#4117 = CYLINDRICAL_SURFACE ( 'NONE', #4675, 17.50000000000000355 ) ;
#4118 = EDGE_LOOP ( 'NONE', ( #3902, #6955, #3792, #2319 ) ) ;
#4119 = EDGE_CURVE ( 'NONE', #4682, #3053, #6745, .T. ) ;
#4120 = CARTESIAN_POINT ( 'NONE',  ( 190.0000000000000000, -12.50000000000000000, 21.65063509461096913 ) ) ;
#4121 = ORIENTED_EDGE ( 'NONE', *, *, #7065, .T. ) ;
#4122 = CARTESIAN_POINT ( 'NONE',  ( -9.381941874331412023, -16.24999999999999645, 7.500000000000000000 ) ) ;
#4123 = ORIENTED_EDGE ( 'NONE', *, *, #6160, .F. ) ;
#4124 = DIRECTION ( 'NONE',  ( 0.000000000000000000, 0.000000000000000000, 1.000000000000000000 ) ) ;
#4125 = FACE_OUTER_BOUND ( 'NONE', #6993, .T. ) ;
#4126 = VERTEX_POINT ( 'NONE', #1184 ) ;
#4127 = ORIENTED_EDGE ( 'NONE', *, *, #3988, .F. ) ;
#4128 = FACE_BOUND ( 'NONE', #4503, .T. ) ;
#4129 = DIRECTION ( 'NONE',  ( 0.000000000000000000, 0.000000000000000000, -1.000000000000000000 ) ) ;
#4130 = CARTESIAN_POINT ( 'NONE',  ( -6.945033096338293890E-14, 144.9999999999998295, 0.000000000000000000 ) ) ;
#4131 = DIRECTION ( 'NONE',  ( 1.000000000000000000, -1.232595164407830946E-32, -1.710569414459005214E-48 ) ) ;
#4132 = PRODUCT_RELATED_PRODUCT_CATEGORY ( 'part', '', ( #1995 ) ) ;
#4133 = DIRECTION ( 'NONE',  ( 1.000000000000000000, 0.000000000000000000, 0.000000000000000000 ) ) ;
#4134 = EDGE_CURVE ( 'NONE', #393, #7515, #5193, .T. ) ;
#4135 = MANIFOLD_SOLID_BREP ( 'Yükseklik-Ekstrüzyon1', #3253 ) ;
#4136 = CARTESIAN_POINT ( 'NONE',  ( -12.49999999999996803, 225.0000000000000284, 0.000000000000000000 ) ) ;
#4137 = CARTESIAN_POINT ( 'NONE',  ( 244.2840207499967278, 217.1990734970208337, 178.2402661832445006 ) ) ;
#4138 = ORIENTED_EDGE ( 'NONE', *, *, #4792, .T. ) ;
#4139 = LINE ( 'NONE', #1664, #3190 ) ;
#4140 = PLANE ( 'NONE',  #3520 ) ;
#4141 = CARTESIAN_POINT ( 'NONE',  ( 314.1025403784437344, 82.50000000000004263, 125.0000000000000000 ) ) ;
#4142 = ORIENTED_EDGE ( 'NONE', *, *, #6320, .T. ) ;
#4143 = EDGE_CURVE ( 'NONE', #5638, #1872, #5464, .T. ) ;
#4144 = ADVANCED_FACE ( 'NONE', ( #1417 ), #139, .T. ) ;
#4145 = CIRCLE ( 'NONE', #180, 12.50000000000000355 ) ;
#4146 = EDGE_LOOP ( 'NONE', ( #2283, #7808, #1284, #918 ) ) ;
#4147 = ORIENTED_EDGE ( 'NONE', *, *, #3412, .T. ) ;
#4148 = CARTESIAN_POINT ( 'NONE',  ( 42.50000000000000711, 187.5000000000000000, 12.50000000000000000 ) ) ;
#4150 = DIRECTION ( 'NONE',  ( -1.000000000000000000, 0.000000000000000000, 0.000000000000000000 ) ) ;
#4149 = AXIS2_PLACEMENT_3D ( 'NONE', #6909, #41, #7506 ) ;
#4151 = AXIS2_PLACEMENT_3D ( 'NONE', #4660, #4546, #7763 ) ;
#4152 = VECTOR ( 'NONE', #3627, 1000.000000000000000 ) ;
#4153 = ORIENTED_EDGE ( 'NONE', *, *, #6796, .T. ) ;
#4154 = DIRECTION ( 'NONE',  ( -1.000000000000000000, 0.000000000000000000, 0.000000000000000000 ) ) ;
#4155 = AXIS2_PLACEMENT_3D ( 'NONE', #2684, #2802, #5240 ) ;
#4156 = VECTOR ( 'NONE', #5669, 1000.000000000000000 ) ;
#4157 = EDGE_LOOP ( 'NONE', ( #3742, #2722, #5549, #6059 ) ) ;
#4158 = FACE_OUTER_BOUND ( 'NONE', #3135, .T. ) ;
#4159 = ORIENTED_EDGE ( 'NONE', *, *, #5576, .F. ) ;
#4160 = CARTESIAN_POINT ( 'NONE',  ( 365.8982392568397017, -18.07018020958731697, 8.577132482464245200 ) ) ;
#4161 = ORIENTED_EDGE ( 'NONE', *, *, #1897, .F. ) ;
#4162 = DIRECTION ( 'NONE',  ( -0.000000000000000000, 0.000000000000000000, -1.000000000000000000 ) ) ;
#4163 = CIRCLE ( 'NONE', #5314, 12.50000000000000000 ) ;
#4164 = LINE ( 'NONE', #3572, #5444 ) ;
#4165 = EDGE_CURVE ( 'NONE', #5042, #2998, #208, .T. ) ;
#4166 = ORIENTED_EDGE ( 'NONE', *, *, #7702, .F. ) ;
#4167 = AXIS2_PLACEMENT_3D ( 'NONE', #2842, #3991, #7642 ) ;
#4168 = ORIENTED_EDGE ( 'NONE', *, *, #311, .F. ) ;
#4169 = FACE_BOUND ( 'NONE', #5529, .T. ) ;
#4170 = FACE_OUTER_BOUND ( 'NONE', #4146, .T. ) ;
#4171 = DIRECTION ( 'NONE',  ( -0.000000000000000000, 0.000000000000000000, -1.000000000000000000 ) ) ;
#4172 = CARTESIAN_POINT ( 'NONE',  ( 412.5000000000000568, 150.0000000000000284, 20.00000000000000000 ) ) ;
#4173 = CARTESIAN_POINT ( 'NONE',  ( 387.5015236343236893, 20.00095227047670576, -0.8223324121160918709 ) ) ;
#4174 = MANIFOLD_SOLID_BREP ( 'Yükseklik-Ekstrüzyon1', #938 ) ;
#4175 = DIRECTION ( 'NONE',  ( -1.000000000000000000, -0.000000000000000000, -0.000000000000000000 ) ) ;
#4176 = VECTOR ( 'NONE', #5137, 1000.000000000000000 ) ;
#4177 = APPLICATION_PROTOCOL_DEFINITION ( 'draft international standard', 'automotive_design', 1998, #694 ) ;
#4178 = CARTESIAN_POINT ( 'NONE',  ( -74.28095588234631919, 12.70544120911856112, 12.50000000000000000 ) ) ;
#4179 = DIRECTION ( 'NONE',  ( -0.000000000000000000, 0.000000000000000000, 1.000000000000000000 ) ) ;
#4180 =( REPRESENTATION_RELATIONSHIP ('NONE','NONE', #6292, #7467 ) REPRESENTATION_RELATIONSHIP_WITH_TRANSFORMATION ( #5165 )SHAPE_REPRESENTATION_RELATIONSHIP( ) );
#4181 = DIRECTION ( 'NONE',  ( 0.000000000000000000, 0.000000000000000000, -1.000000000000000000 ) ) ;
#4182 = ORIENTED_EDGE ( 'NONE', *, *, #5071, .T. ) ;
#4183 = EDGE_LOOP ( 'NONE', ( #4958, #2367 ) ) ;
#4184 = EDGE_LOOP ( 'NONE', ( #2639, #1669, #3734, #7281 ) ) ;
#4185 = ADVANCED_FACE ( 'NONE', ( #2058 ), #3230, .F. ) ;
#4186 = DIRECTION ( 'NONE',  ( 0.000000000000000000, 0.000000000000000000, 1.000000000000000000 ) ) ;
#4187 = ORIENTED_EDGE ( 'NONE', *, *, #3517, .F. ) ;
#4188 = FACE_OUTER_BOUND ( 'NONE', #7451, .T. ) ;
#4189 = DIRECTION ( 'NONE',  ( 0.000000000000000000, 0.000000000000000000, -1.000000000000000000 ) ) ;
#4190 = CIRCLE ( 'NONE', #7407, 12.50000000000000000 ) ;
#4191 = CARTESIAN_POINT ( 'NONE',  ( 0.000000000000000000, 0.000000000000000000, 90.00000000000000000 ) ) ;
#4192 = ADVANCED_FACE ( 'NONE', ( #1903 ), #4345, .T. ) ;
#4193 = ORIENTED_EDGE ( 'NONE', *, *, #7721, .F. ) ;
#4194 = CARTESIAN_POINT ( 'NONE',  ( 41.25000000000002842, 47.50000000000003553, 17.50000000000000000 ) ) ;
#4195 = AXIS2_PLACEMENT_3D ( 'NONE', #6942, #6263, #2692 ) ;
#4196 = VECTOR ( 'NONE', #4465, 1000.000000000000000 ) ;
#4197 = EDGE_CURVE ( 'NONE', #6483, #1563, #1304, .T. ) ;
#4198 = ORIENTED_EDGE ( 'NONE', *, *, #4457, .F. ) ;
#4199 = CARTESIAN_POINT ( 'NONE',  ( 279.9038105676658006, 161.6025403784438765, 12.50000000000000000 ) ) ;
#4200 = ORIENTED_EDGE ( 'NONE', *, *, #2206, .F. ) ;
#4201 = CARTESIAN_POINT ( 'NONE',  ( 363.1810740285039287, -19.58130419088990948, -4.090982884146981746 ) ) ;
#4202 = ORIENTED_EDGE ( 'NONE', *, *, #4306, .T. ) ;
#4203 = CARTESIAN_POINT ( 'NONE',  ( -37.50000000000000000, 4.592427351555481498E-15, 12.50000000000000000 ) ) ;
#4204 = AXIS2_PLACEMENT_3D ( 'NONE', #7436, #89, #7907 ) ;
#4205 = DIRECTION ( 'NONE',  ( 0.000000000000000000, 0.000000000000000000, 1.000000000000000000 ) ) ;
#4206 = EDGE_LOOP ( 'NONE', ( #451, #5261, #1740, #6197 ) ) ;
#4207 = VECTOR ( 'NONE', #5777, 1000.000000000000000 ) ;
#4208 = VECTOR ( 'NONE', #4327, 1000.000000000000000 ) ;
#4209 = ADVANCED_BREP_SHAPE_REPRESENTATION ( '', ( #1743, #5785 ), #4233 ) ;
#4210 = EDGE_LOOP ( 'NONE', ( #1996, #3010, #952, #1041 ) ) ;
#4211 = EDGE_CURVE ( 'NONE', #6240, #7248, #5642, .T. ) ;
#4212 = CARTESIAN_POINT ( 'NONE',  ( -11.78095584970496290, 62.70544120911855401, 12.50000000000000000 ) ) ;
#4213 = DIRECTION ( 'NONE',  ( 1.000000000000000000, 0.000000000000000000, 0.000000000000000000 ) ) ;
#4214 = CARTESIAN_POINT ( 'NONE',  ( 279.9038105676658006, 161.6025403784438765, 12.50000000000000000 ) ) ;
#4215 = DIRECTION ( 'NONE',  ( -0.000000000000000000, -0.000000000000000000, -1.000000000000000000 ) ) ;
#4216 = LINE ( 'NONE', #7830, #1206 ) ;
#4217 = LINE ( 'NONE', #6669, #1347 ) ;
#4218 = EDGE_CURVE ( 'NONE', #1637, #345, #1488, .T. ) ;
#4219 = DIRECTION ( 'NONE',  ( -4.789677997474686366E-16, -1.000000000000000000, -0.000000000000000000 ) ) ;
#4220 = SHAPE_DEFINITION_REPRESENTATION ( #2710, #949 ) ;
#4221 = DIRECTION ( 'NONE',  ( -4.789677997474686366E-16, -1.000000000000000000, 0.000000000000000000 ) ) ;
#4222 = DIRECTION ( 'NONE',  ( 0.000000000000000000, 0.000000000000000000, -1.000000000000000000 ) ) ;
#4223 = DIRECTION ( 'NONE',  ( -0.000000000000000000, -0.000000000000000000, -1.000000000000000000 ) ) ;
#4224 = DIRECTION ( 'NONE',  ( -0.000000000000000000, -0.000000000000000000, -1.000000000000000000 ) ) ;
#4225 = PRODUCT_DEFINITION_CONTEXT ( 'detailed design', #6434, 'design' ) ;
#4226 = ORIENTED_EDGE ( 'NONE', *, *, #2581, .T. ) ;
#4227 = ORIENTED_EDGE ( 'NONE', *, *, #5158, .F. ) ;
#4228 = LINE ( 'NONE', #5479, #2644 ) ;
#4229 = CARTESIAN_POINT ( 'NONE',  ( 314.1025403784437344, 75.00000000000005684, 125.0000000000000000 ) ) ;
#4230 = FACE_OUTER_BOUND ( 'NONE', #2211, .T. ) ;
#4231 = FILL_AREA_STYLE ('',( #2395 ) ) ;
#4232 = ORIENTED_EDGE ( 'NONE', *, *, #4704, .T. ) ;
#4233 =( GEOMETRIC_REPRESENTATION_CONTEXT ( 3 ) GLOBAL_UNCERTAINTY_ASSIGNED_CONTEXT ( ( #5841 ) ) GLOBAL_UNIT_ASSIGNED_CONTEXT ( ( #1029, #2278, #2234 ) ) REPRESENTATION_CONTEXT ( 'NONE', 'WORKASPACE' ) );
#4234 = DIRECTION ( 'NONE',  ( 0.000000000000000000, -0.000000000000000000, 1.000000000000000000 ) ) ;
#4235 = EDGE_CURVE ( 'NONE', #3303, #1519, #5467, .T. ) ;
#4236 = EDGE_CURVE ( 'NONE', #4609, #3444, #700, .T. ) ;
#4237 = ORIENTED_EDGE ( 'NONE', *, *, #2901, .F. ) ;
#4238 = CARTESIAN_POINT ( 'NONE',  ( 12.50000000000000000, 0.000000000000000000, 35.78244274809159720 ) ) ;
#4239 = EDGE_LOOP ( 'NONE', ( #902, #7572, #4052, #7592, #6079, #6172 ) ) ;
#4240 = CARTESIAN_POINT ( 'NONE',  ( 369.4067717504701704, -16.58082631454064781, 11.18611842067925011 ) ) ;
#4241 = ORIENTED_EDGE ( 'NONE', *, *, #5859, .T. ) ;
#4242 = DIRECTION ( 'NONE',  ( -1.000000000000000000, 0.000000000000000000, 0.000000000000000000 ) ) ;
#4243 = ADVANCED_FACE ( 'NONE', ( #6921 ), #216, .F. ) ;
#4244 = DIRECTION ( 'NONE',  ( 0.000000000000000000, 0.000000000000000000, -1.000000000000000000 ) ) ;
#4245 = EDGE_CURVE ( 'NONE', #5178, #3850, #6620, .T. ) ;
#4246 = VERTEX_POINT ( 'NONE', #4511 ) ;
#4247 = ORIENTED_EDGE ( 'NONE', *, *, #1890, .F. ) ;
#4248 = ORIENTED_EDGE ( 'NONE', *, *, #7721, .T. ) ;
#4249 = PRODUCT_DEFINITION_SHAPE ( 'NONE', 'NONE',  #7931 ) ;
#4250 = CARTESIAN_POINT ( 'NONE',  ( 325.0000000000000000, 0.000000000000000000, 0.000000000000000000 ) ) ;
#4251 = ADVANCED_FACE ( 'NONE', ( #7558 ), #4504, .F. ) ;
#4252 = CARTESIAN_POINT ( 'NONE',  ( 41.25000000000002842, 177.6587708172407076, 12.50000000000000000 ) ) ;
#4253 = CARTESIAN_POINT ( 'NONE',  ( 340.0000000000000000, 12.50000000000000000, 21.65063509461096913 ) ) ;
#4254 = LINE ( 'NONE', #614, #2074 ) ;
#4255 = DIRECTION ( 'NONE',  ( 0.5000000000000003331, -0.8660254037844384856, 0.000000000000000000 ) ) ;
#4256 = DIRECTION ( 'NONE',  ( -0.000000000000000000, -0.000000000000000000, 1.000000000000000000 ) ) ;
#4257 = DIRECTION ( 'NONE',  ( 1.000000000000000000, 9.251858538542979716E-16, 0.000000000000000000 ) ) ;
#4258 = PLANE ( 'NONE',  #4456 ) ;
#4259 = DIRECTION ( 'NONE',  ( -0.000000000000000000, -0.000000000000000000, 1.000000000000000000 ) ) ;
#4260 = VECTOR ( 'NONE', #3140, 1000.000000000000227 ) ;
#4261 = DIRECTION ( 'NONE',  ( -1.000000000000000000, 4.789677997474686366E-16, -0.000000000000000000 ) ) ;
#4262 = EDGE_CURVE ( 'NONE', #2065, #1547, #5221, .T. ) ;
#4263 = ORIENTED_EDGE ( 'NONE', *, *, #5910, .F. ) ;
#4264 = CARTESIAN_POINT ( 'NONE',  ( 6.602357126051254174E-16, 0.000000000000000000, -31.78244274809162562 ) ) ;
#4265 = DIRECTION ( 'NONE',  ( 0.7070068166729618353, 0.7072067315700302226, 0.000000000000000000 ) ) ;
#4266 = DIRECTION ( 'NONE',  ( 1.000000000000000000, 0.000000000000000000, 0.000000000000000000 ) ) ;
#4267 = CARTESIAN_POINT ( 'NONE',  ( -18.76388374866283471, 7.854341805648601650E-17, 7.500000000000000000 ) ) ;
#4268 = ORIENTED_EDGE ( 'NONE', *, *, #7101, .F. ) ;
#4269 = AXIS2_PLACEMENT_3D ( 'NONE', #2864, #5256, #4058 ) ;
#4270 = PLANE ( 'NONE',  #2896 ) ;
#4271 = CLOSED_SHELL ( 'NONE', ( #2939, #3143, #24, #644, #2832, #2136, #6166, #4676, #1898, #4587, #6081 ) ) ;
#4272 = VERTEX_POINT ( 'NONE', #1498 ) ;
#4273 = AXIS2_PLACEMENT_3D ( 'NONE', #766, #6265, #248 ) ;
#4274 = CARTESIAN_POINT ( 'NONE',  ( 0.000000000000000000, 0.000000000000000000, 200.0000000000000000 ) ) ;
#4275 = MECHANICAL_DESIGN_GEOMETRIC_PRESENTATION_REPRESENTATION (  '', ( #7743 ), #5558 ) ;
#4276 = VERTEX_POINT ( 'NONE', #4657 ) ;
#4277 = VECTOR ( 'NONE', #2669, 1000.000000000000000 ) ;
#4278 = CARTESIAN_POINT ( 'NONE',  ( 372.0966397287041900, -15.87504132268115242, 12.16528391369894990 ) ) ;
#4279 = ORIENTED_EDGE ( 'NONE', *, *, #7066, .T. ) ;
#4280 = SURFACE_STYLE_FILL_AREA ( #4800 ) ;
#4281 = DIRECTION ( 'NONE',  ( -0.000000000000000000, 0.000000000000000000, -1.000000000000000000 ) ) ;
#4282 = VECTOR ( 'NONE', #5935, 1000.000000000000000 ) ;
#4283=STYLED_ITEM('',(#7969),#1475);
#4284 = ORIENTED_EDGE ( 'NONE', *, *, #6111, .T. ) ;
#4285 = ORIENTED_EDGE ( 'NONE', *, *, #7575, .T. ) ;
#4286 = EDGE_CURVE ( 'NONE', #3124, #5409, #2275, .T. ) ;
#4287 = AXIS2_PLACEMENT_3D ( 'NONE', #1044, #6855, #3096 ) ;
#4288 = EDGE_LOOP ( 'NONE', ( #3774, #2054 ) ) ;
#4289 = LINE ( 'NONE', #4212, #1889 ) ;
#4290 = CARTESIAN_POINT ( 'NONE',  ( 385.1226161722381107, -18.60597098153023055, -7.344632615169738088 ) ) ;
#4291 = LINE ( 'NONE', #4854, #2811 ) ;
#4292 = CARTESIAN_POINT ( 'NONE',  ( 400.0000000000000000, 12.50000000000000000, 25.00000000000000000 ) ) ;
#4293 = EDGE_CURVE ( 'NONE', #819, #1936, #2705, .T. ) ;
#4294 = LINE ( 'NONE', #3856, #6713 ) ;
#4295 = CIRCLE ( 'NONE', #3665, 20.00000000000000000 ) ;
#4296 = DIRECTION ( 'NONE',  ( 0.5000000000000003331, -0.8660254037844384856, 0.000000000000000000 ) ) ;
#4297 = DIRECTION ( 'NONE',  ( -0.000000000000000000, -0.000000000000000000, -1.000000000000000000 ) ) ;
#4298 = FACE_OUTER_BOUND ( 'NONE', #6783, .T. ) ;
#4300 = DIRECTION ( 'NONE',  ( -1.000000000000000000, 0.000000000000000000, 0.000000000000000000 ) ) ;
#4299 = AXIS2_PLACEMENT_3D ( 'NONE', #4858, #4256, #6540 ) ;
#4301 = FACE_OUTER_BOUND ( 'NONE', #2204, .T. ) ;
#4302 = VERTEX_POINT ( 'NONE', #895 ) ;
#4303 = AXIS2_PLACEMENT_3D ( 'NONE', #4786, #3633, #3556 ) ;
#4304 =( NAMED_UNIT ( * ) SI_UNIT ( $, .STERADIAN. ) SOLID_ANGLE_UNIT ( ) );
#4305 = ORIENTED_EDGE ( 'NONE', *, *, #6653, .T. ) ;
#4306 = EDGE_CURVE ( 'NONE', #7818, #36, #3906, .T. ) ;
#4307 = DIRECTION ( 'NONE',  ( -4.789677997474686366E-16, -1.000000000000000000, 0.000000000000000000 ) ) ;
#4308 = PLANE ( 'NONE',  #4969 ) ;
#4309 = DIRECTION ( 'NONE',  ( -0.7072067315700303336, 0.7070068166729619463, 0.000000000000000000 ) ) ;
#4310 = CYLINDRICAL_SURFACE ( 'NONE', #448, 24.99999998367932719 ) ;
#4311 = ORIENTED_EDGE ( 'NONE', *, *, #1211, .T. ) ;
#4312 = TOROIDAL_SURFACE ( 'NONE', #2130, 13.00000000000000178, 0.5000000000000000000 ) ;
#4313 = DIRECTION ( 'NONE',  ( -1.000000000000000000, 0.000000000000000000, 0.000000000000000000 ) ) ;
#4314 = AXIS2_PLACEMENT_3D ( 'NONE', #2087, #4646, #7109 ) ;
#4315 = CARTESIAN_POINT ( 'NONE',  ( 375.0000000000000000, 15.61249499599599488, 12.50000000000000711 ) ) ;
#4316 = VERTEX_POINT ( 'NONE', #7593 ) ;
#4317 = CARTESIAN_POINT ( 'NONE',  ( 367.6834352059303797, -17.23925164521633846, -10.14275924251023220 ) ) ;
#4318 = ORIENTED_EDGE ( 'NONE', *, *, #5774, .T. ) ;
#4319 = LINE ( 'NONE', #6176, #6339 ) ;
#4320 = CIRCLE ( 'NONE', #7904, 15.00000000000000000 ) ;
#4322 = ORIENTED_EDGE ( 'NONE', *, *, #4053, .F. ) ;
#4321 = EDGE_CURVE ( 'NONE', #4446, #5884, #5341, .T. ) ;
#4323 = EDGE_LOOP ( 'NONE', ( #2733, #5759, #2674, #4089, #2671 ) ) ;
#4324 = ORIENTED_EDGE ( 'NONE', *, *, #5969, .T. ) ;
#4325 = DIRECTION ( 'NONE',  ( -0.000000000000000000, -0.000000000000000000, -1.000000000000000000 ) ) ;
#4326 = CARTESIAN_POINT ( 'NONE',  ( 387.0651080012848411, -19.73086988975742528, 3.295070860296623216 ) ) ;
#4327 = DIRECTION ( 'NONE',  ( -1.000000000000000000, -0.000000000000000000, -0.000000000000000000 ) ) ;
#4328 = CARTESIAN_POINT ( 'NONE',  ( 0.000000000000000000, 47.50000000000009237, 0.000000000000000000 ) ) ;
#4329 = DIRECTION ( 'NONE',  ( 1.224646799147353207E-16, 1.000000000000000000, -0.000000000000000000 ) ) ;
#4330 = AXIS2_PLACEMENT_3D ( 'NONE', #5794, #6918, #2137 ) ;
#4331 = EDGE_CURVE ( 'NONE', #109, #5450, #7632, .T. ) ;
#4332 = VECTOR ( 'NONE', #6913, 1000.000000000000000 ) ;
#4333 =( REPRESENTATION_RELATIONSHIP ('NONE','NONE', #6292, #1772 ) REPRESENTATION_RELATIONSHIP_WITH_TRANSFORMATION ( #5544 )SHAPE_REPRESENTATION_RELATIONSHIP( ) );
#4334 = EDGE_CURVE ( 'NONE', #556, #2226, #2829, .T. ) ;
#4335 = CIRCLE ( 'NONE', #7418, 17.50000000000000355 ) ;
#4336 = CARTESIAN_POINT ( 'NONE',  ( 340.0000000000000000, 25.00000000000000000, 0.000000000000000000 ) ) ;
#4337 = CARTESIAN_POINT ( 'NONE',  ( -25.00000000000000000, 0.000000000000000000, 0.000000000000000000 ) ) ;
#4338 = AXIS2_PLACEMENT_3D ( 'NONE', #3619, #1289, #123 ) ;
#4339 = DIRECTION ( 'NONE',  ( 1.000000000000000000, 0.000000000000000000, 0.000000000000000000 ) ) ;
#4340 = DIRECTION ( 'NONE',  ( 0.000000000000000000, 0.000000000000000000, 1.000000000000000000 ) ) ;
#4341 = ADVANCED_FACE ( 'NONE', ( #3308 ), #2097, .F. ) ;
#4342 = ADVANCED_FACE ( 'NONE', ( #421 ), #4312, .T. ) ;
#4343 = VERTEX_POINT ( 'NONE', #4581 ) ;
#4344 = ORIENTED_EDGE ( 'NONE', *, *, #7240, .F. ) ;
#4345 = CYLINDRICAL_SURFACE ( 'NONE', #4953, 35.78244274809159720 ) ;
#4346 = FACE_OUTER_BOUND ( 'NONE', #7306, .T. ) ;
#4347 = CARTESIAN_POINT ( 'NONE',  ( 25.00000000000000000, 0.000000000000000000, 0.000000000000000000 ) ) ;
#4348 = CARTESIAN_POINT ( 'NONE',  ( 162.5000000000000000, 1.990051048614448997E-14, 0.000000000000000000 ) ) ;
#4349 = VERTEX_POINT ( 'NONE', #5263 ) ;
#4350 = EDGE_CURVE ( 'NONE', #1859, #1477, #6365, .T. ) ;
#4351 = CARTESIAN_POINT ( 'NONE',  ( 42.50000000000000711, 187.5000000000000000, 0.000000000000000000 ) ) ;
#4352 = MANIFOLD_SOLID_BREP ( 'Pah1', #2480 ) ;
#4353 = CARTESIAN_POINT ( 'NONE',  ( 38.21904415029484170, 19.40417101989674009, 12.50000000000000000 ) ) ;
#4354 = ORIENTED_EDGE ( 'NONE', *, *, #1207, .T. ) ;
#4355 = DIRECTION ( 'NONE',  ( -1.000000000000000000, 0.000000000000000000, 0.000000000000000000 ) ) ;
#4356 = EDGE_LOOP ( 'NONE', ( #2800, #5977, #2633, #4529 ) ) ;
#4357 = PRESENTATION_STYLE_ASSIGNMENT (( #604 ) ) ;
#4358 = CARTESIAN_POINT ( 'NONE',  ( 0.000000000000000000, 0.000000000000000000, 2.500000000000085265 ) ) ;
#4359 = EDGE_CURVE ( 'NONE', #5929, #3389, #5875, .T. ) ;
#4360 = EDGE_LOOP ( 'NONE', ( #6370, #2103, #296, #1416 ) ) ;
#4361 = MANIFOLD_SOLID_BREP ( 'Radyus3', #7351 ) ;
#4362 = ORIENTED_EDGE ( 'NONE', *, *, #3755, .T. ) ;
#4363 = ORIENTED_EDGE ( 'NONE', *, *, #126, .F. ) ;
#4364 = DIRECTION ( 'NONE',  ( 0.000000000000000000, 1.000000000000000000, -0.000000000000000000 ) ) ;
#4365 = CARTESIAN_POINT ( 'NONE',  ( 386.8183406672370666, -19.58094920198549360, 4.092816503359988367 ) ) ;
#4366 = CARTESIAN_POINT ( 'NONE',  ( 0.000000000000000000, 0.000000000000000000, 0.000000000000000000 ) ) ;
#4367 = FACE_OUTER_BOUND ( 'NONE', #22, .T. ) ;
#4368 = DIRECTION ( 'NONE',  ( -1.000000000000000000, 0.000000000000000000, 0.000000000000000000 ) ) ;
#4369 = SHAPE_DEFINITION_REPRESENTATION ( #205, #2073 ) ;
#4370 = CARTESIAN_POINT ( 'NONE',  ( 412.4999999999998295, 145.0000000000000284, 0.000000000000000000 ) ) ;
#4371 = CARTESIAN_POINT ( 'NONE',  ( 0.000000000000000000, 187.5000000000000000, 12.50000000000000000 ) ) ;
#4372 = CARTESIAN_POINT ( 'NONE',  ( 46.25000000000002842, 144.7499999999999147, 130.0000000000000000 ) ) ;
#4373 = DIRECTION ( 'NONE',  ( -1.000000000000000000, 0.000000000000000000, 0.000000000000000000 ) ) ;
#4374 = ORIENTED_EDGE ( 'NONE', *, *, #395, .T. ) ;
#4375 =( NAMED_UNIT ( * ) PLANE_ANGLE_UNIT ( ) SI_UNIT ( $, .RADIAN. ) );
#4376 = VERTEX_POINT ( 'NONE', #4102 ) ;
#4377 = EDGE_CURVE ( 'NONE', #4623, #4115, #4432, .T. ) ;
#4378 = CARTESIAN_POINT ( 'NONE',  ( 296.6025403784439050, 80.00000000000007105, 5.000000000000000000 ) ) ;
#4379 = DIRECTION ( 'NONE',  ( -0.000000000000000000, -0.000000000000000000, -1.000000000000000000 ) ) ;
#4380 = DIRECTION ( 'NONE',  ( 0.000000000000000000, 0.000000000000000000, -1.000000000000000000 ) ) ;
#4381 = DIRECTION ( 'NONE',  ( 1.000000000000000000, 0.000000000000000000, 0.000000000000000000 ) ) ;
#4382 = VERTEX_POINT ( 'NONE', #2913 ) ;
#4383 = EDGE_CURVE ( 'NONE', #4671, #2143, #5980, .T. ) ;
#4384 = DIRECTION ( 'NONE',  ( -1.000000000000000000, 0.000000000000000000, 0.000000000000000000 ) ) ;
#4385 = ORIENTED_EDGE ( 'NONE', *, *, #251, .T. ) ;
#4386 = EDGE_CURVE ( 'NONE', #957, #7913, #5075, .T. ) ;
#4387 = CARTESIAN_POINT ( 'NONE',  ( 362.5200448844577750, 19.98745133777255134, 0.8232361438305751955 ) ) ;
#4388 = ORIENTED_EDGE ( 'NONE', *, *, #1283, .F. ) ;
#4389 = LINE ( 'NONE', #6852, #5972 ) ;
#4391 = ORIENTED_EDGE ( 'NONE', *, *, #6695, .F. ) ;
#4390 = AXIS2_PLACEMENT_3D ( 'NONE', #6793, #6915, #3897 ) ;
#4392 = AXIS2_PLACEMENT_3D ( 'NONE', #1067, #5398, #433 ) ;
#4393 = LINE ( 'NONE', #6250, #2817 ) ;
#4394 = DIRECTION ( 'NONE',  ( -0.000000000000000000, -0.000000000000000000, -1.000000000000000000 ) ) ;
#4395 = EDGE_CURVE ( 'NONE', #2517, #3524, #2954, .T. ) ;
#4396 = ORIENTED_EDGE ( 'NONE', *, *, #1834, .T. ) ;
#4397 = AXIS2_PLACEMENT_3D ( 'NONE', #6559, #4179, #2346 ) ;
#4398 = ORIENTED_EDGE ( 'NONE', *, *, #803, .T. ) ;
#4399 = EDGE_LOOP ( 'NONE', ( #851, #1278, #3455, #7343 ) ) ;
#4400 = CARTESIAN_POINT ( 'NONE',  ( -12.50000000000000000, 0.000000000000000000, 0.000000000000000000 ) ) ;
#4401 = EDGE_CURVE ( 'NONE', #4126, #1302, #1366, .T. ) ;
#4402 = CARTESIAN_POINT ( 'NONE',  ( 187.5000000000000000, 0.000000000000000000, 12.50000000000000000 ) ) ;
#4403 = CARTESIAN_POINT ( 'NONE',  ( 52.50000000000000711, 0.000000000000000000, 5.000000000000000000 ) ) ;
#4404 = ORIENTED_EDGE ( 'NONE', *, *, #7404, .T. ) ;
#4405 = AXIS2_PLACEMENT_3D ( 'NONE', #5521, #2061, #3233 ) ;
#4406 = AXIS2_PLACEMENT_3D ( 'NONE', #1412, #5790, #3300 ) ;
#4407 = CARTESIAN_POINT ( 'NONE',  ( 0.000000000000000000, 177.4999999999999432, 0.000000000000000000 ) ) ;
#4408 = AXIS2_PLACEMENT_3D ( 'NONE', #2720, #6490, #3880 ) ;
#4409 = AXIS2_PLACEMENT_3D ( 'NONE', #5298, #891, #5132 ) ;
#4410 = CONTEXT_DEPENDENT_SHAPE_REPRESENTATION ( #6951, #4756 ) ;
#4411 = CARTESIAN_POINT ( 'NONE',  ( 412.5000000000000568, 80.00000000000001421, 5.000000000000000000 ) ) ;
#4412 = DIRECTION ( 'NONE',  ( 0.000000000000000000, -0.000000000000000000, -1.000000000000000000 ) ) ;
#4413 = DIRECTION ( 'NONE',  ( 0.000000000000000000, -0.000000000000000000, -1.000000000000000000 ) ) ;
#4414 = DIRECTION ( 'NONE',  ( -0.000000000000000000, -1.000000000000000000, -0.000000000000000000 ) ) ;
#4415 = CIRCLE ( 'NONE', #196, 15.00000000000000000 ) ;
#4416 = ORIENTED_EDGE ( 'NONE', *, *, #5562, .T. ) ;
#4417 = DIRECTION ( 'NONE',  ( 1.000000000000000000, 4.789677997474691297E-16, 0.000000000000000000 ) ) ;
#4418 = AXIS2_PLACEMENT_3D ( 'NONE', #1595, #4042, #6496 ) ;
#4419 = ORIENTED_EDGE ( 'NONE', *, *, #6379, .F. ) ;
#4420 = DIRECTION ( 'NONE',  ( -1.000000000000000000, -0.000000000000000000, -0.000000000000000000 ) ) ;
#4421 = DIRECTION ( 'NONE',  ( 2.960594732333750117E-15, -1.000000000000000000, 0.000000000000000000 ) ) ;
#4422 = CARTESIAN_POINT ( 'NONE',  ( -25.00000000000000000, 1.530808498934191521E-15, 12.50000000000000000 ) ) ;
#4423 = LINE ( 'NONE', #1421, #6980 ) ;
#4424 = ORIENTED_EDGE ( 'NONE', *, *, #6661, .T. ) ;
#4425 = CARTESIAN_POINT ( 'NONE',  ( 378.3097126640965939, 15.95485291322333588, 12.06092292949322520 ) ) ;
#4426 = VECTOR ( 'NONE', #4866, 1000.000000000000000 ) ;
#4427 = EDGE_CURVE ( 'NONE', #4926, #6165, #2381, .T. ) ;
#4428 = EDGE_CURVE ( 'NONE', #30, #1382, #7277, .T. ) ;
#4429 = CARTESIAN_POINT ( 'NONE',  ( 370.9032405149421834, 16.13643827696138189, -11.81688677216110861 ) ) ;
#4430 = VERTEX_POINT ( 'NONE', #3670 ) ;
#4431 = DIRECTION ( 'NONE',  ( 0.000000000000000000, -1.000000000000000000, 0.000000000000000000 ) ) ;
#4432 = CIRCLE ( 'NONE', #482, 31.78244274809162562 ) ;
#4433 = VERTEX_POINT ( 'NONE', #6790 ) ;
#4434 = LINE ( 'NONE', #6892, #105 ) ;
#4435 = CARTESIAN_POINT ( 'NONE',  ( -15.64999999999999680, 0.000000000000000000, 200.0000000000000000 ) ) ;
#4436 = ADVANCED_FACE ( 'NONE', ( #6191 ), #6752, .F. ) ;
#4437 = AXIS2_PLACEMENT_3D ( 'NONE', #4495, #2172, #5904 ) ;
#4438 = ORIENTED_EDGE ( 'NONE', *, *, #6757, .T. ) ;
#4439 = FACE_OUTER_BOUND ( 'NONE', #4463, .T. ) ;
#4440 = ORIENTED_EDGE ( 'NONE', *, *, #718, .F. ) ;
#4441 = ORIENTED_EDGE ( 'NONE', *, *, #385, .T. ) ;
#4442 = DIRECTION ( 'NONE',  ( 0.000000000000000000, 0.000000000000000000, -1.000000000000000000 ) ) ;
#4443 = LINE ( 'NONE', #4402, #617 ) ;
#4444 = LINE ( 'NONE', #4403, #7548 ) ;
#4446 = VERTEX_POINT ( 'NONE', #163 ) ;
#4445 = CIRCLE ( 'NONE', #2927, 12.50000000000000000 ) ;
#4447 = DIRECTION ( 'NONE',  ( -1.000000000000000000, 0.000000000000000000, 0.000000000000000000 ) ) ;
#4448 = ADVANCED_FACE ( 'NONE', ( #2613 ), #7356, .F. ) ;
#4449 = VECTOR ( 'NONE', #1118, 1000.000000000000000 ) ;
#4450 = CIRCLE ( 'NONE', #2021, 12.50000000000000000 ) ;
#4451 = DIRECTION ( 'NONE',  ( -0.000000000000000000, 0.000000000000000000, 1.000000000000000000 ) ) ;
#4452 = DIRECTION ( 'NONE',  ( -0.000000000000000000, 0.000000000000000000, 1.000000000000000000 ) ) ;
#4453 = DIRECTION ( 'NONE',  ( 0.000000000000000000, 0.000000000000000000, 1.000000000000000000 ) ) ;
#4454 = FACE_OUTER_BOUND ( 'NONE', #6300, .T. ) ;
#4455 = MECHANICAL_DESIGN_GEOMETRIC_PRESENTATION_REPRESENTATION (  '', ( #4714 ), #2155 ) ;
#4456 = AXIS2_PLACEMENT_3D ( 'NONE', #4371, #1370, #4412 ) ;
#4457 = EDGE_CURVE ( 'NONE', #1583, #3990, #983, .T. ) ;
#4458 = VERTEX_POINT ( 'NONE', #4370 ) ;
#4459 =( LENGTH_UNIT ( ) NAMED_UNIT ( * ) SI_UNIT ( .MILLI., .METRE. ) );
#4460 = CIRCLE ( 'NONE', #1520, 65.50000000000000000 ) ;
#4461 = CIRCLE ( 'NONE', #3583, 12.50000000000000000 ) ;
#4462 = DIRECTION ( 'NONE',  ( 0.000000000000000000, 0.000000000000000000, 1.000000000000000000 ) ) ;
#4463 = EDGE_LOOP ( 'NONE', ( #7415, #469, #4226, #4374 ) ) ;
#4464 = DIRECTION ( 'NONE',  ( 1.000000000000000000, 0.000000000000000000, 0.000000000000000000 ) ) ;
#4465 = DIRECTION ( 'NONE',  ( -1.295260195396012743E-15, -1.000000000000000000, 0.000000000000000000 ) ) ;
#4466 = CARTESIAN_POINT ( 'NONE',  ( 0.000000000000000000, 0.000000000000000000, 200.0000000000000000 ) ) ;
#4467 = DIRECTION ( 'NONE',  ( 1.000000000000000000, 0.000000000000000000, 0.000000000000000000 ) ) ;
#4468 = ORIENTED_EDGE ( 'NONE', *, *, #1011, .T. ) ;
#4469 = UNCERTAINTY_MEASURE_WITH_UNIT (LENGTH_MEASURE( 1.000000000000000082E-05 ), #1858, 'distance_accuracy_value', 'NONE');
#4470 = ORIENTED_EDGE ( 'NONE', *, *, #4980, .T. ) ;
#4471 = CARTESIAN_POINT ( 'NONE',  ( -31.24999999999997158, 0.000000000000000000, 195.5000000000000000 ) ) ;
#4472 = ORIENTED_EDGE ( 'NONE', *, *, #7246, .T. ) ;
#4473 = DIRECTION ( 'NONE',  ( -0.000000000000000000, -0.000000000000000000, -1.000000000000000000 ) ) ;
#4474 = VERTEX_POINT ( 'NONE', #1851 ) ;
#4475 = PRODUCT_DEFINITION ( 'UNKNOWN', '', #7705, #5110 ) ;
#4476 = FACE_OUTER_BOUND ( 'NONE', #4069, .T. ) ;
#4477 = CARTESIAN_POINT ( 'NONE',  ( -1.301042606982605321E-15, -37.50000000000000000, 0.000000000000000000 ) ) ;
#4478 = EDGE_CURVE ( 'NONE', #1918, #7209, #212, .T. ) ;
#4479 = EDGE_LOOP ( 'NONE', ( #77, #3647 ) ) ;
#4480 = DIRECTION ( 'NONE',  ( -0.000000000000000000, -0.000000000000000000, -1.000000000000000000 ) ) ;
#4481 = ORIENTED_EDGE ( 'NONE', *, *, #7893, .T. ) ;
#4482 = EDGE_CURVE ( 'NONE', #3593, #3005, #5730, .T. ) ;
#4483 = VERTEX_POINT ( 'NONE', #88 ) ;
#4484 = CARTESIAN_POINT ( 'NONE',  ( 42.50000000000000711, 182.5000000000000000, 0.000000000000000000 ) ) ;
#4485 = ADVANCED_FACE ( 'NONE', ( #1257, #1966 ), #2538, .T. ) ;
#4486 =( LENGTH_UNIT ( ) NAMED_UNIT ( * ) SI_UNIT ( .MILLI., .METRE. ) );
#4487 = CARTESIAN_POINT ( 'NONE',  ( 399.3518360003419048, 12.50000000000000000, -13.85262921941844816 ) ) ;
#4488 = ORIENTED_EDGE ( 'NONE', *, *, #1311, .T. ) ;
#4489 = LINE ( 'NONE', #4607, #2102 ) ;
#4490 = ADVANCED_BREP_SHAPE_REPRESENTATION ( '', ( #4352, #5785 ), #1803 ) ;
#4491 = EDGE_CURVE ( 'NONE', #5961, #6561, #1505, .T. ) ;
#4492 = PRODUCT_DEFINITION_SHAPE ( 'NONE', 'NONE',  #3304 ) ;
#4493 = CONTEXT_DEPENDENT_SHAPE_REPRESENTATION ( #7719, #4249 ) ;
#4494 = AXIS2_PLACEMENT_3D ( 'NONE', #6518, #541, #4655 ) ;
#4495 = CARTESIAN_POINT ( 'NONE',  ( 13.00000000000000178, 0.000000000000000000, 0.5000000000000004441 ) ) ;
#4496 = DIRECTION ( 'NONE',  ( 1.000000000000000000, 0.000000000000000000, 0.000000000000000000 ) ) ;
#4497 = CARTESIAN_POINT ( 'NONE',  ( -74.28095588234631919, -62.29455879088143888, 0.000000000000000000 ) ) ;
#4498 = LINE ( 'NONE', #4988, #936 ) ;
#4499 = EDGE_CURVE ( 'NONE', #5649, #6617, #6369, .T. ) ;
#4500 = VERTEX_POINT ( 'NONE', #6152 ) ;
#4501 = CARTESIAN_POINT ( 'NONE',  ( 0.000000000000000000, 0.000000000000000000, 90.00000000000000000 ) ) ;
#4502 = DIRECTION ( 'NONE',  ( -4.789593822244058314E-16, -1.000000000000000000, -5.328524673440537306E-22 ) ) ;
#4503 = EDGE_LOOP ( 'NONE', ( #2920, #1060 ) ) ;
#4504 = CYLINDRICAL_SURFACE ( 'NONE', #7136, 12.49999999999999467 ) ;
#4505 = CARTESIAN_POINT ( 'NONE',  ( 2.775557561562891351E-14, 225.0000000000000284, 0.000000000000000000 ) ) ;
#4506 = DIRECTION ( 'NONE',  ( -1.295260195396012940E-15, 1.000000000000000000, 0.000000000000000000 ) ) ;
#4507 = ADVANCED_FACE ( 'NONE', ( #6912 ), #5590, .F. ) ;
#4508 = CARTESIAN_POINT ( 'NONE',  ( 0.000000000000000000, 0.000000000000000000, -18.75000000000009948 ) ) ;
#4509 = EDGE_LOOP ( 'NONE', ( #7123, #7777 ) ) ;
#4510 = EDGE_LOOP ( 'NONE', ( #4847, #722, #1706, #266, #3872, #1286, #396 ) ) ;
#4511 = CARTESIAN_POINT ( 'NONE',  ( -37.49999999999989342, 187.4999999999999432, 12.50000000000000000 ) ) ;
#4512 = ORIENTED_EDGE ( 'NONE', *, *, #7829, .T. ) ;
#4513 = DIRECTION ( 'NONE',  ( 0.000000000000000000, 0.000000000000000000, 1.000000000000000000 ) ) ;
#4514 = VERTEX_POINT ( 'NONE', #7507 ) ;
#4515 = DIRECTION ( 'NONE',  ( 0.000000000000000000, 0.000000000000000000, -1.000000000000000000 ) ) ;
#4516 = DIRECTION ( 'NONE',  ( 3.469446951953614189E-17, 1.000000000000000000, -0.000000000000000000 ) ) ;
#4517 = AXIS2_PLACEMENT_3D ( 'NONE', #6702, #3662, #124 ) ;
#4518 = ORIENTED_EDGE ( 'NONE', *, *, #4014, .T. ) ;
#4519 = DIRECTION ( 'NONE',  ( 0.000000000000000000, -1.481552359947913884E-16, 1.000000000000000000 ) ) ;
#4520 = EDGE_LOOP ( 'NONE', ( #2390, #522, #3463, #5396 ) ) ;
#4521 = AXIS2_PLACEMENT_3D ( 'NONE', #2965, #1789, #3483 ) ;
#4522 = EDGE_LOOP ( 'NONE', ( #5982, #7554 ) ) ;
#4523 = DIRECTION ( 'NONE',  ( 1.295260195396013137E-15, -1.000000000000000000, 0.000000000000000000 ) ) ;
#4524 = SURFACE_STYLE_FILL_AREA ( #5741 ) ;
#4525 = DIRECTION ( 'NONE',  ( 0.000000000000000000, 0.000000000000000000, 1.000000000000000000 ) ) ;
#4526 = CIRCLE ( 'NONE', #5945, 25.00000000000000000 ) ;
#4527 = SHAPE_REPRESENTATION ( 'Rod', ( #5785 ), #536 ) ;
#4528 = EDGE_CURVE ( 'NONE', #5938, #7297, #731, .T. ) ;
#4529 = ORIENTED_EDGE ( 'NONE', *, *, #3517, .T. ) ;
#4530 = AXIS2_PLACEMENT_3D ( 'NONE', #652, #3781, #7546 ) ;
#4531 = EDGE_CURVE ( 'NONE', #1859, #2637, #655, .T. ) ;
#4532 = CIRCLE ( 'NONE', #2497, 32.75000000000000000 ) ;
#4533 = AXIS2_PLACEMENT_3D ( 'NONE', #890, #3937, #3821 ) ;
#4534 = CARTESIAN_POINT ( 'NONE',  ( 6.602357126051254174E-16, 4.137156037882910601E-15, 31.78244274809162562 ) ) ;
#4535 = DIRECTION ( 'NONE',  ( -1.000000000000000000, -0.000000000000000000, -0.000000000000000000 ) ) ;
#4536 = DIRECTION ( 'NONE',  ( 0.000000000000000000, -0.000000000000000000, 1.000000000000000000 ) ) ;
#4537 = CARTESIAN_POINT ( 'NONE',  ( 12.50000000000000000, 0.000000000000000000, 0.000000000000000000 ) ) ;
#4538 = CIRCLE ( 'NONE', #1086, 20.00000000000000000 ) ;
#4539 = CIRCLE ( 'NONE', #2366, 12.50000000000000355 ) ;
#4540 = VERTEX_POINT ( 'NONE', #3786 ) ;
#4541 =( NAMED_UNIT ( * ) PLANE_ANGLE_UNIT ( ) SI_UNIT ( $, .RADIAN. ) );
#4542 = ORIENTED_EDGE ( 'NONE', *, *, #3988, .T. ) ;
#4543 = CARTESIAN_POINT ( 'NONE',  ( 138.5360707071662887, -22.21662272193747256, 25.00000000000000000 ) ) ;
#4545 = CYLINDRICAL_SURFACE ( 'NONE', #6331, 5.000000000000000888 ) ;
#4544 = AXIS2_PLACEMENT_3D ( 'NONE', #3977, #5947, #2133 ) ;
#4546 = DIRECTION ( 'NONE',  ( 0.000000000000000000, -0.000000000000000000, -1.000000000000000000 ) ) ;
#4547 = VERTEX_POINT ( 'NONE', #3860 ) ;
#4548 = VECTOR ( 'NONE', #2678, 1000.000000000000000 ) ;
#4549 = ORIENTED_EDGE ( 'NONE', *, *, #1322, .F. ) ;
#4550 = EDGE_CURVE ( 'NONE', #1497, #2024, #3109, .T. ) ;
#4551 = LINE ( 'NONE', #825, #398 ) ;
#4552 = EDGE_LOOP ( 'NONE', ( #3352, #4716, #2968, #2248 ) ) ;
#4553 = DIRECTION ( 'NONE',  ( 0.000000000000000000, 0.000000000000000000, -1.000000000000000000 ) ) ;
#4554 = CARTESIAN_POINT ( 'NONE',  ( -27.08354679051374347, 177.4999999999999432, 12.55124306091976649 ) ) ;
#4555 = CARTESIAN_POINT ( 'NONE',  ( -20.00000000000000000, 0.000000000000000000, 45.00000000000000000 ) ) ;
#4556 = AXIS2_PLACEMENT_3D ( 'NONE', #2432, #4751, #1227 ) ;
#4557 = FACE_OUTER_BOUND ( 'NONE', #7410, .T. ) ;
#4558 = PRODUCT_DEFINITION_SHAPE ( 'NONE', 'NONE',  #7921 ) ;
#4559 = ORIENTED_EDGE ( 'NONE', *, *, #2242, .F. ) ;
#4560 = CYLINDRICAL_SURFACE ( 'NONE', #757, 20.00000000000000000 ) ;
#4561 = ORIENTED_EDGE ( 'NONE', *, *, #6000, .F. ) ;
#4562 = EDGE_LOOP ( 'NONE', ( #7890, #713 ) ) ;
#4563 = FACE_OUTER_BOUND ( 'NONE', #6492, .T. ) ;
#4564 = DIRECTION ( 'NONE',  ( 0.000000000000000000, 0.000000000000000000, 1.000000000000000000 ) ) ;
#4565 = DIRECTION ( 'NONE',  ( -0.000000000000000000, -0.000000000000000000, -1.000000000000000000 ) ) ;
#4566 = AXIS2_PLACEMENT_3D ( 'NONE', #7585, #3973, #923 ) ;
#4567 = VERTEX_POINT ( 'NONE', #6305 ) ;
#4568 = CIRCLE ( 'NONE', #6887, 5.000000000000004441 ) ;
#4569 = FACE_OUTER_BOUND ( 'NONE', #1944, .T. ) ;
#4570 = CARTESIAN_POINT ( 'NONE',  ( 187.5000000000000000, 0.000000000000000000, 12.50000000000000000 ) ) ;
#4571 = DIRECTION ( 'NONE',  ( -0.000000000000000000, -0.000000000000000000, -1.000000000000000000 ) ) ;
#4572 = CARTESIAN_POINT ( 'NONE',  ( 326.6025403784437913, 75.00000000000005684, 125.0000000000000000 ) ) ;
#4573 = ADVANCED_FACE ( 'NONE', ( #3186 ), #6269, .F. ) ;
#4574 = FACE_OUTER_BOUND ( 'NONE', #3754, .T. ) ;
#4575 = AXIS2_PLACEMENT_3D ( 'NONE', #7142, #1561, #962 ) ;
#4576 = AXIS2_PLACEMENT_3D ( 'NONE', #3947, #896, #6037 ) ;
#4577 = EDGE_CURVE ( 'NONE', #389, #6926, #5709, .T. ) ;
#4578 = CARTESIAN_POINT ( 'NONE',  ( 0.000000000000000000, 0.000000000000000000, 0.000000000000000000 ) ) ;
#4579 = ORIENTED_EDGE ( 'NONE', *, *, #862, .F. ) ;
#4580 = COLOUR_RGB ( '',0.7921568627450980005, 0.8196078431372548767, 0.9333333333333333481 ) ;
#4581 = CARTESIAN_POINT ( 'NONE',  ( -27.49999999999989342, 177.4999999999999432, 12.65877081724072362 ) ) ;
#4582 = CARTESIAN_POINT ( 'NONE',  ( -37.49999999999995026, 47.50000000000009237, 12.50000000000000000 ) ) ;
#4583 = AXIS2_PLACEMENT_3D ( 'NONE', #1024, #5305, #2914 ) ;
#4584 = DIRECTION ( 'NONE',  ( 1.000000000000000000, -4.789677997474686366E-16, -0.000000000000000000 ) ) ;
#4585 = ADVANCED_FACE ( 'NONE', ( #2499 ), #3464, .F. ) ;
#4586 = ORIENTED_EDGE ( 'NONE', *, *, #1066, .T. ) ;
#4587 = ADVANCED_FACE ( 'NONE', ( #4569 ), #5205, .T. ) ;
#4588 = AXIS2_PLACEMENT_3D ( 'NONE', #793, #5508, #6899 ) ;
#4589 = AXIS2_PLACEMENT_3D ( 'NONE', #4985, #1817, #3110 ) ;
#4590 =( REPRESENTATION_RELATIONSHIP ('NONE','NONE', #6292, #341 ) REPRESENTATION_RELATIONSHIP_WITH_TRANSFORMATION ( #887 )SHAPE_REPRESENTATION_RELATIONSHIP( ) );
#4591 = EDGE_LOOP ( 'NONE', ( #1351, #2929 ) ) ;
#4592 = DIRECTION ( 'NONE',  ( -0.000000000000000000, 0.000000000000000000, 1.000000000000000000 ) ) ;
#4593 = ORIENTED_EDGE ( 'NONE', *, *, #7360, .T. ) ;
#4594 = DIRECTION ( 'NONE',  ( -0.4585571717133501424, 0.8886649088774988270, 0.000000000000000000 ) ) ;
#4595 = ORIENTED_EDGE ( 'NONE', *, *, #2358, .T. ) ;
#4596 = DIRECTION ( 'NONE',  ( -1.000000000000000000, 0.000000000000000000, 0.000000000000000000 ) ) ;
#4597 = AXIS2_PLACEMENT_3D ( 'NONE', #2982, #3579, #5905 ) ;
#4598 = LINE ( 'NONE', #4477, #2755 ) ;
#4599 = ORIENTED_EDGE ( 'NONE', *, *, #273, .T. ) ;
#4600 = FACE_OUTER_BOUND ( 'NONE', #3979, .T. ) ;
#4601 = VERTEX_POINT ( 'NONE', #2777 ) ;
#4602 = DIRECTION ( 'NONE',  ( -0.000000000000000000, -0.000000000000000000, -1.000000000000000000 ) ) ;
#4603 = VERTEX_POINT ( 'NONE', #3935 ) ;
#4604 = DIRECTION ( 'NONE',  ( 1.000000000000000000, 0.000000000000000000, 0.000000000000000000 ) ) ;
#4605 = CARTESIAN_POINT ( 'NONE',  ( -9.381941874331412023, -16.24999999999999645, 0.000000000000000000 ) ) ;
#4606 = LINE ( 'NONE', #3458, #4449 ) ;
#4607 = CARTESIAN_POINT ( 'NONE',  ( 17.50000000000000355, 2.143131898507868643E-15, 97.50000000000000000 ) ) ;
#4608 = ADVANCED_FACE ( 'NONE', ( #3418 ), #2214, .F. ) ;
#4609 = VERTEX_POINT ( 'NONE', #888 ) ;
#4610 = DIRECTION ( 'NONE',  ( -0.000000000000000000, -0.000000000000000000, -1.000000000000000000 ) ) ;
#4611 = LINE ( 'NONE', #925, #7866 ) ;
#4612 = LINE ( 'NONE', #7070, #1327 ) ;
#4613 = CARTESIAN_POINT ( 'NONE',  ( 384.3729953227158944, 18.20868245435311295, 8.279865652961362343 ) ) ;
#4614 = CARTESIAN_POINT ( 'NONE',  ( 12.50000000000000000, 0.000000000000000000, 0.000000000000000000 ) ) ;
#4615 =( NAMED_UNIT ( * ) SI_UNIT ( $, .STERADIAN. ) SOLID_ANGLE_UNIT ( ) );
#4616 = VERTEX_POINT ( 'NONE', #2695 ) ;
#4617 = DIRECTION ( 'NONE',  ( 1.000000000000000000, 0.000000000000000000, 0.000000000000000000 ) ) ;
#4618 = LINE ( 'NONE', #5721, #7026 ) ;
#4619 = DIRECTION ( 'NONE',  ( 0.000000000000000000, 0.000000000000000000, 1.000000000000000000 ) ) ;
#4620 = CARTESIAN_POINT ( 'NONE',  ( 326.6025403784438481, 150.0000000000000568, 125.0000000000000000 ) ) ;
#4621 = EDGE_LOOP ( 'NONE', ( #4440, #1756, #1285, #7545 ) ) ;
#4622 = AXIS2_PLACEMENT_3D ( 'NONE', #2309, #2380, #7200 ) ;
#4623 = VERTEX_POINT ( 'NONE', #4534 ) ;
#4624 = ORIENTED_EDGE ( 'NONE', *, *, #4165, .F. ) ;
#4625 = EDGE_CURVE ( 'NONE', #3331, #1336, #1606, .T. ) ;
#4626 = DIRECTION ( 'NONE',  ( 1.000000000000000000, 0.000000000000000000, 0.000000000000000000 ) ) ;
#4627 = ORIENTED_EDGE ( 'NONE', *, *, #3219, .F. ) ;
#4628 = DIRECTION ( 'NONE',  ( 0.000000000000000000, -0.000000000000000000, 1.000000000000000000 ) ) ;
#4629 = CYLINDRICAL_SURFACE ( 'NONE', #6196, 5.000000000000004441 ) ;
#4630 = ADVANCED_FACE ( 'NONE', ( #2049 ), #5208, .T. ) ;
#4631 = ORIENTED_EDGE ( 'NONE', *, *, #3513, .F. ) ;
#4632 =( LENGTH_UNIT ( ) NAMED_UNIT ( * ) SI_UNIT ( .MILLI., .METRE. ) );
#4633 = LINE ( 'NONE', #5116, #702 ) ;
#4634 = EDGE_CURVE ( 'NONE', #603, #155, #7521, .T. ) ;
#4635 = ORIENTED_EDGE ( 'NONE', *, *, #6061, .T. ) ;
#4636 = CARTESIAN_POINT ( 'NONE',  ( 0.000000000000000000, 0.000000000000000000, 1.000000000000028644 ) ) ;
#4637 = ORIENTED_EDGE ( 'NONE', *, *, #1181, .T. ) ;
#4638 = LINE ( 'NONE', #4001, #4805 ) ;
#4639 = ORIENTED_EDGE ( 'NONE', *, *, #967, .T. ) ;
#4640 = FACE_OUTER_BOUND ( 'NONE', #7771, .T. ) ;
#4641 =( NAMED_UNIT ( * ) SI_UNIT ( $, .STERADIAN. ) SOLID_ANGLE_UNIT ( ) );
#4642 = CYLINDRICAL_SURFACE ( 'NONE', #5213, 12.50000000000000355 ) ;
#4643 = FACE_OUTER_BOUND ( 'NONE', #3036, .T. ) ;
#4644 = EDGE_LOOP ( 'NONE', ( #1344, #3914, #3289, #4279, #6221, #6920, #4324, #2114, #2607, #4111 ) ) ;
#4645 = EDGE_CURVE ( 'NONE', #1, #4927, #3297, .T. ) ;
#4646 = DIRECTION ( 'NONE',  ( 0.000000000000000000, 0.000000000000000000, 1.000000000000000000 ) ) ;
#4647 = LINE ( 'NONE', #1653, #6141 ) ;
#4648 = CARTESIAN_POINT ( 'NONE',  ( -31.24999999999997158, 111.9999999999999289, 130.0000000000000000 ) ) ;
#4649 = VECTOR ( 'NONE', #808, 1000.000000000000000 ) ;
#4650 = AXIS2_PLACEMENT_3D ( 'NONE', #3443, #5888, #392 ) ;
#4651 = DIRECTION ( 'NONE',  ( -1.000000000000000000, -0.000000000000000000, -0.000000000000000000 ) ) ;
#4652 = CARTESIAN_POINT ( 'NONE',  ( 387.3259369069866693, 19.89156578813670251, 2.119594365942482739 ) ) ;
#4653 = CIRCLE ( 'NONE', #4782, 32.75000000000000000 ) ;
#4654 = DIRECTION ( 'NONE',  ( 1.000000000000000000, 0.000000000000000000, 0.000000000000000000 ) ) ;
#4655 = DIRECTION ( 'NONE',  ( 0.4714459106766391017, -2.257459899895315222E-16, 0.8818949786149563597 ) ) ;
#4656 = EDGE_LOOP ( 'NONE', ( #2330, #5802, #4783, #4247 ) ) ;
#4657 = CARTESIAN_POINT ( 'NONE',  ( 17.32050807568877104, -2.500000000000002220, 0.000000000000000000 ) ) ;
#4658 = CARTESIAN_POINT ( 'NONE',  ( 340.0000000000000000, 12.50000000000000000, 0.000000000000000000 ) ) ;
#4659 = FACE_OUTER_BOUND ( 'NONE', #6687, .T. ) ;
#4660 = CARTESIAN_POINT ( 'NONE',  ( -27.49999999999994671, 42.50000000000009237, 12.50000000000000000 ) ) ;
#4661 = VERTEX_POINT ( 'NONE', #7067 ) ;
#4662 = VECTOR ( 'NONE', #284, 1000.000000000000114 ) ;
#4663 = COLOUR_RGB ( '',0.7921568627450980005, 0.8196078431372548767, 0.9333333333333333481 ) ;
#4664 = AXIS2_PLACEMENT_3D ( 'NONE', #1853, #6754, #3188 ) ;
#4665 = ORIENTED_EDGE ( 'NONE', *, *, #7805, .T. ) ;
#4666 = VECTOR ( 'NONE', #71, 1000.000000000000000 ) ;
#4667 = CIRCLE ( 'NONE', #2609, 5.000000000000000000 ) ;
#4668 = ORIENTED_EDGE ( 'NONE', *, *, #3809, .T. ) ;
#4669 = DIRECTION ( 'NONE',  ( -0.000000000000000000, -0.000000000000000000, -1.000000000000000000 ) ) ;
#4670 = DIRECTION ( 'NONE',  ( 1.000000000000000000, 0.000000000000000000, 0.000000000000000000 ) ) ;
#4671 = VERTEX_POINT ( 'NONE', #5129 ) ;
#4672 = DIRECTION ( 'NONE',  ( -1.000000000000000000, 0.000000000000000000, 0.000000000000000000 ) ) ;
#4673 = DIRECTION ( 'NONE',  ( -0.000000000000000000, -0.000000000000000000, -1.000000000000000000 ) ) ;
#4674 = EDGE_CURVE ( 'NONE', #2808, #7266, #1494, .T. ) ;
#4675 = AXIS2_PLACEMENT_3D ( 'NONE', #6536, #3004, #1035 ) ;
#4676 = ADVANCED_FACE ( 'NONE', ( #411 ), #6383, .T. ) ;
#4677 = ORIENTED_EDGE ( 'NONE', *, *, #7449, .F. ) ;
#4678 = CARTESIAN_POINT ( 'NONE',  ( 41.25000000000002842, 177.5000000000000000, 12.50000000000000000 ) ) ;
#4679 = VERTEX_POINT ( 'NONE', #4054 ) ;
#4680 = DIRECTION ( 'NONE',  ( 0.000000000000000000, 0.000000000000000000, 1.000000000000000000 ) ) ;
#4681 = AXIS2_PLACEMENT_3D ( 'NONE', #5032, #1989, #1914 ) ;
#4682 = VERTEX_POINT ( 'NONE', #1443 ) ;
#4683 = DIRECTION ( 'NONE',  ( -1.000000000000000000, 0.000000000000000000, 0.000000000000000000 ) ) ;
#4684 = DIRECTION ( 'NONE',  ( -0.000000000000000000, -0.000000000000000000, -1.000000000000000000 ) ) ;
#4685 = ADVANCED_FACE ( 'NONE', ( #6463 ), #6504, .T. ) ;
#4686 = LINE ( 'NONE', #2975, #3144 ) ;
#4687 = VERTEX_POINT ( 'NONE', #7622 ) ;
#4688 = EDGE_LOOP ( 'NONE', ( #187, #472, #5272, #7824, #6497 ) ) ;
#4689 = PLANE ( 'NONE',  #6626 ) ;
#4690 = CARTESIAN_POINT ( 'NONE',  ( 325.0000000000000000, 12.50000000000000000, 21.65063509461096913 ) ) ;
#4692 = CARTESIAN_POINT ( 'NONE',  ( 0.000000000000000000, 111.9999999999999289, 130.0000000000000000 ) ) ;
#4691 = VECTOR ( 'NONE', #7317, 1000.000000000000000 ) ;
#4693 = CARTESIAN_POINT ( 'NONE',  ( 0.000000000000000000, 0.000000000000000000, 0.000000000000000000 ) ) ;
#4694 = CARTESIAN_POINT ( 'NONE',  ( -17.99038105676657651, 1.734723475976807094E-15, 7.500000000000000000 ) ) ;
#4695 = CARTESIAN_POINT ( 'NONE',  ( 0.000000000000000000, 0.000000000000000000, 12.50000000000000000 ) ) ;
#4696 = APPLICATION_PROTOCOL_DEFINITION ( 'draft international standard', 'automotive_design', 1998, #6846 ) ;
#4697 = VERTEX_POINT ( 'NONE', #1012 ) ;
#4698 = DIRECTION ( 'NONE',  ( 0.000000000000000000, 1.000000000000000000, 0.000000000000000000 ) ) ;
#4699 = CARTESIAN_POINT ( 'NONE',  ( -9.381941874331415576, 16.25000000000000000, 7.500000000000000000 ) ) ;
#4700 = CYLINDRICAL_SURFACE ( 'NONE', #5432, 12.50000000000000355 ) ;
#4701 = SURFACE_STYLE_FILL_AREA ( #6478 ) ;
#4702 = EDGE_LOOP ( 'NONE', ( #5492, #1953, #6334, #2062 ) ) ;
#4703 = VECTOR ( 'NONE', #5623, 1000.000000000000000 ) ;
#4704 = EDGE_CURVE ( 'NONE', #2195, #556, #2400, .T. ) ;
#4705 = ORIENTED_EDGE ( 'NONE', *, *, #1994, .T. ) ;
#4706 = EDGE_LOOP ( 'NONE', ( #1579, #1122, #2448, #4624 ) ) ;
#4707 = AXIS2_PLACEMENT_3D ( 'NONE', #4994, #2509, #4906 ) ;
#4708 = EDGE_LOOP ( 'NONE', ( #795, #4263, #3481, #7174 ) ) ;
#4709 = FACE_OUTER_BOUND ( 'NONE', #7255, .T. ) ;
#4710 = CARTESIAN_POINT ( 'NONE',  ( 0.000000000000000000, 0.000000000000000000, 49.99999999999998579 ) ) ;
#4711 = EDGE_LOOP ( 'NONE', ( #5023, #7689, #3569, #670, #4091, #6571 ) ) ;
#4712 = SURFACE_STYLE_USAGE ( .BOTH. , #7690 ) ;
#4713 = LINE ( 'NONE', #7179, #1604 ) ;
#4714=STYLED_ITEM('',(#7948),#7010);
#4715 = CIRCLE ( 'NONE', #7420, 25.00000000000002132 ) ;
#4716 = ORIENTED_EDGE ( 'NONE', *, *, #2600, .T. ) ;
#4717 = DIRECTION ( 'NONE',  ( 0.000000000000000000, 0.000000000000000000, 1.000000000000000000 ) ) ;
#4718 = EDGE_LOOP ( 'NONE', ( #4870, #7417, #1782, #6473, #3216 ) ) ;
#4719 = CONICAL_SURFACE ( 'NONE', #4588, 12.50000000000000000, 0.7853981633974491672 ) ;
#4720 = PRODUCT_DEFINITION ( 'UNKNOWN', '', #5128, #7282 ) ;
#4721 = CYLINDRICAL_SURFACE ( 'NONE', #6482, 12.50000000000000000 ) ;
#4722 = AXIS2_PLACEMENT_3D ( 'NONE', #5667, #6625, #7859 ) ;
#4723 = VERTEX_POINT ( 'NONE', #847 ) ;
#4724 = FACE_OUTER_BOUND ( 'NONE', #5701, .T. ) ;
#4725 = ADVANCED_FACE ( 'NONE', ( #6425 ), #3298, .T. ) ;
#4726 = CARTESIAN_POINT ( 'NONE',  ( -37.50000000000000000, 4.592427351555481498E-15, 0.000000000000000000 ) ) ;
#4727 = ORIENTED_EDGE ( 'NONE', *, *, #6944, .T. ) ;
#4728 = EDGE_CURVE ( 'NONE', #481, #6592, #5749, .T. ) ;
#4729 = VERTEX_POINT ( 'NONE', #5825 ) ;
#4730 = EDGE_CURVE ( 'NONE', #4039, #221, #2922, .T. ) ;
#4731 = DIRECTION ( 'NONE',  ( 1.000000000000000000, 0.000000000000000000, 0.000000000000000000 ) ) ;
#4732 = FACE_OUTER_BOUND ( 'NONE', #4184, .T. ) ;
#4733 = FACE_OUTER_BOUND ( 'NONE', #1188, .T. ) ;
#4734 = EDGE_CURVE ( 'NONE', #2643, #4927, #6665, .T. ) ;
#4735 = FACE_OUTER_BOUND ( 'NONE', #1972, .T. ) ;
#4736 = CARTESIAN_POINT ( 'NONE',  ( 387.1693935999242058, 19.79494591053120445, -2.886379146895018177 ) ) ;
#4737 = EDGE_CURVE ( 'NONE', #5360, #698, #4766, .T. ) ;
#4738 = EDGE_CURVE ( 'NONE', #6273, #1167, #5941, .T. ) ;
#4739 = CARTESIAN_POINT ( 'NONE',  ( 296.6025403784437913, 0.000000000000000000, 0.000000000000000000 ) ) ;
#4740 = DIRECTION ( 'NONE',  ( 4.789593822244094799E-16, 1.000000000000000000, 5.328524654824031087E-22 ) ) ;
#4741 = ORIENTED_EDGE ( 'NONE', *, *, #231, .F. ) ;
#4742 = DIRECTION ( 'NONE',  ( 0.000000000000000000, 0.000000000000000000, -1.000000000000000000 ) ) ;
#4743 = CARTESIAN_POINT ( 'NONE',  ( 0.000000000000000000, 0.000000000000000000, 195.9999999999999716 ) ) ;
#4744 = DIRECTION ( 'NONE',  ( 1.000000000000000000, 0.000000000000000000, -0.000000000000000000 ) ) ;
#4745 = CARTESIAN_POINT ( 'NONE',  ( 12.50000000000000355, 0.000000000000000000, 0.000000000000000000 ) ) ;
#4746 = ORIENTED_EDGE ( 'NONE', *, *, #4645, .T. ) ;
#4747 = AXIS2_PLACEMENT_3D ( 'NONE', #2149, #7047, #1424 ) ;
#4748 = ORIENTED_EDGE ( 'NONE', *, *, #3565, .F. ) ;
#4749 = ORIENTED_EDGE ( 'NONE', *, *, #4499, .F. ) ;
#4750 = ADVANCED_FACE ( 'NONE', ( #5414 ), #6581, .T. ) ;
#4751 = DIRECTION ( 'NONE',  ( -0.000000000000000000, -0.000000000000000000, -1.000000000000000000 ) ) ;
#4752 = CARTESIAN_POINT ( 'NONE',  ( 400.0000000000000000, 12.50000000000000000, -12.95183384698871620 ) ) ;
#4753 =( GEOMETRIC_REPRESENTATION_CONTEXT ( 3 ) GLOBAL_UNCERTAINTY_ASSIGNED_CONTEXT ( ( #2228 ) ) GLOBAL_UNIT_ASSIGNED_CONTEXT ( ( #1696, #7712, #5423 ) ) REPRESENTATION_CONTEXT ( 'NONE', 'WORKASPACE' ) );
#4754 = VERTEX_POINT ( 'NONE', #4252 ) ;
#4755 = DIRECTION ( 'NONE',  ( -0.9335804380297003657, 0.3583679195021128305, 0.000000000000000000 ) ) ;
#4756 = PRODUCT_DEFINITION_SHAPE ( 'NONE', 'NONE',  #7926 ) ;
#4757 = ORIENTED_EDGE ( 'NONE', *, *, #2841, .F. ) ;
#4758 = DIRECTION ( 'NONE',  ( -0.000000000000000000, -0.000000000000000000, -1.000000000000000000 ) ) ;
#4759 = ORIENTED_EDGE ( 'NONE', *, *, #5069, .T. ) ;
#4760 = DIRECTION ( 'NONE',  ( 1.000000000000000000, 0.000000000000000000, 0.000000000000000000 ) ) ;
#4761 = ORIENTED_EDGE ( 'NONE', *, *, #1061, .F. ) ;
#4762 = CARTESIAN_POINT ( 'NONE',  ( 17.32050807568877104, -2.500000000000002220, 7.500000000000000000 ) ) ;
#4763 = DIRECTION ( 'NONE',  ( 0.000000000000000000, -0.000000000000000000, 1.000000000000000000 ) ) ;
#4764 = ORIENTED_EDGE ( 'NONE', *, *, #1449, .T. ) ;
#4765 = ORIENTED_EDGE ( 'NONE', *, *, #803, .F. ) ;
#4766 = LINE ( 'NONE', #456, #4824 ) ;
#4767 = CARTESIAN_POINT ( 'NONE',  ( 0.000000000000000000, 0.000000000000000000, 75.00000000000000000 ) ) ;
#4768 = CARTESIAN_POINT ( 'NONE',  ( 12.50000000000000000, 0.000000000000000000, 0.000000000000000000 ) ) ;
#4769 = LINE ( 'NONE', #6703, #6324 ) ;
#4770 = CARTESIAN_POINT ( 'NONE',  ( 384.9030275854814818, 18.48453940650270866, -7.670107965951052265 ) ) ;
#4771 = EDGE_CURVE ( 'NONE', #6738, #2966, #730, .T. ) ;
#4772 = EDGE_CURVE ( 'NONE', #4729, #1108, #3808, .T. ) ;
#4773 = CARTESIAN_POINT ( 'NONE',  ( 0.7190441666157093570, -30.59582893112819946, 0.000000000000000000 ) ) ;
#4774 = SHAPE_DEFINITION_REPRESENTATION ( #275, #341 ) ;
#4775 = AXIS2_PLACEMENT_3D ( 'NONE', #6941, #2081, #4004 ) ;
#4776 = VECTOR ( 'NONE', #7844, 1000.000000000000000 ) ;
#4777 = SURFACE_STYLE_FILL_AREA ( #3508 ) ;
#4778 = LINE ( 'NONE', #3547, #7915 ) ;
#4779 = LINE ( 'NONE', #7869, #7606 ) ;
#4780 = CARTESIAN_POINT ( 'NONE',  ( 375.0000000000000000, 25.00000000000000000, -12.50000000000000000 ) ) ;
#4781 = ORIENTED_EDGE ( 'NONE', *, *, #5838, .F. ) ;
#4782 = AXIS2_PLACEMENT_3D ( 'NONE', #3118, #6238, #5644 ) ;
#4783 = ORIENTED_EDGE ( 'NONE', *, *, #1911, .T. ) ;
#4784 = VERTEX_POINT ( 'NONE', #6104 ) ;
#4785 = VERTEX_POINT ( 'NONE', #571 ) ;
#4786 = CARTESIAN_POINT ( 'NONE',  ( 412.5000000000000000, 87.50000000000005684, 17.49999999999998934 ) ) ;
#4787 = DIRECTION ( 'NONE',  ( 1.000000000000000000, 0.000000000000000000, 0.000000000000000000 ) ) ;
#4789 = CARTESIAN_POINT ( 'NONE',  ( 4.000000000000004441, 4.382085397712380109E-15, -35.78244274809159720 ) ) ;
#4788 = CIRCLE ( 'NONE', #5564, 24.99999999999999289 ) ;
#4790 = ORIENTED_EDGE ( 'NONE', *, *, #1154, .F. ) ;
#4791 = FACE_OUTER_BOUND ( 'NONE', #5612, .T. ) ;
#4792 = EDGE_CURVE ( 'NONE', #6174, #6926, #492, .T. ) ;
#4793 = CONICAL_SURFACE ( 'NONE', #452, 12.50000000000000000, 0.7853981633974521648 ) ;
#4794 = VECTOR ( 'NONE', #7552, 1000.000000000000000 ) ;
#4795 = ORIENTED_EDGE ( 'NONE', *, *, #6400, .F. ) ;
#4796 = DIRECTION ( 'NONE',  ( -1.000000000000000000, 0.000000000000000000, -0.000000000000000000 ) ) ;
#4797 = EDGE_LOOP ( 'NONE', ( #2924, #2116, #158, #7885 ) ) ;
#4798 = CARTESIAN_POINT ( 'NONE',  ( 362.6740630930135580, -19.89156578813670251, 2.119594365942482739 ) ) ;
#4799 = ORIENTED_EDGE ( 'NONE', *, *, #1283, .T. ) ;
#4800 = FILL_AREA_STYLE ('',( #1240 ) ) ;
#4801 = VECTOR ( 'NONE', #7273, 1000.000000000000000 ) ;
#4802 = DIRECTION ( 'NONE',  ( -1.000000000000000000, 0.000000000000000000, 0.000000000000000000 ) ) ;
#4803 = ADVANCED_FACE ( 'NONE', ( #5460 ), #5604, .T. ) ;
#4804 = EDGE_LOOP ( 'NONE', ( #3306, #2256, #1746, #2754 ) ) ;
#4805 = VECTOR ( 'NONE', #4602, 1000.000000000000000 ) ;
#4806 = EDGE_LOOP ( 'NONE', ( #3955, #6007, #3925, #3062 ) ) ;
#4807 = CARTESIAN_POINT ( 'NONE',  ( 375.0000000000000000, -15.61249499599599488, 12.50000000000000711 ) ) ;
#4808 = CARTESIAN_POINT ( 'NONE',  ( 75.00000000000000000, 10.56842436860067735, 25.00000000000000000 ) ) ;
#4809 = CYLINDRICAL_SURFACE ( 'NONE', #3829, 25.00000000000000000 ) ;
#4810 = CARTESIAN_POINT ( 'NONE',  ( 25.00000000000000000, 0.000000000000000000, -25.00000000000000000 ) ) ;
#4811 = EDGE_CURVE ( 'NONE', #1830, #4661, #2414, .T. ) ;
#4812 = DIRECTION ( 'NONE',  ( 0.000000000000000000, -0.000000000000000000, -1.000000000000000000 ) ) ;
#4813 = AXIS2_PLACEMENT_3D ( 'NONE', #777, #2508, #174 ) ;
#4814 = CARTESIAN_POINT ( 'NONE',  ( 12.50000000000002309, 225.0000000000000284, 12.50000000000000000 ) ) ;
#4815 = CARTESIAN_POINT ( 'NONE',  ( 399.3518360003419048, -12.50000000000000000, 13.85262921941844816 ) ) ;
#4816 = APPLICATION_PROTOCOL_DEFINITION ( 'draft international standard', 'automotive_design', 1998, #6434 ) ;
#4817 = ADVANCED_FACE ( 'NONE', ( #2259 ), #4689, .T. ) ;
#4818 = CARTESIAN_POINT ( 'NONE',  ( 0.000000000000000000, 25.00000000000000000, 25.00000000000000000 ) ) ;
#4819 = FACE_BOUND ( 'NONE', #6055, .T. ) ;
#4820 = DIRECTION ( 'NONE',  ( -1.000000000000000000, 0.000000000000000000, 0.000000000000000000 ) ) ;
#4821 = DIRECTION ( 'NONE',  ( -1.000000000000000000, 0.000000000000000000, 0.000000000000000000 ) ) ;
#4822 = ORIENTED_EDGE ( 'NONE', *, *, #3414, .F. ) ;
#4823 = ADVANCED_FACE ( 'NONE', ( #1652, #4093, #4128, #6546, #4169, #1047 ), #6027, .F. ) ;
#4824 = VECTOR ( 'NONE', #2902, 1000.000000000000000 ) ;
#4825 = EDGE_LOOP ( 'NONE', ( #6537, #2709, #6460, #3728 ) ) ;
#4826 = EDGE_CURVE ( 'NONE', #5884, #4446, #2784, .T. ) ;
#4827 = ORIENTED_EDGE ( 'NONE', *, *, #3123, .F. ) ;
#4828 = EDGE_CURVE ( 'NONE', #6609, #2940, #7899, .T. ) ;
#4829 = CARTESIAN_POINT ( 'NONE',  ( 12.50000000000000355, 0.000000000000000000, -12.50000000000000000 ) ) ;
#4830 = DIRECTION ( 'NONE',  ( 1.000000000000000000, 0.000000000000000000, 0.000000000000000000 ) ) ;
#4831 = AXIS2_PLACEMENT_3D ( 'NONE', #1202, #3703, #6144 ) ;
#4832 = DIRECTION ( 'NONE',  ( -0.000000000000000000, 0.000000000000000000, 1.000000000000000000 ) ) ;
#4833 = SURFACE_STYLE_USAGE ( .BOTH. , #6087 ) ;
#4834 = VERTEX_POINT ( 'NONE', #7826 ) ;
#4835 = CARTESIAN_POINT ( 'NONE',  ( 199.9999999999998863, 262.5000000000000568, 12.50000000000000000 ) ) ;
#4836 = CIRCLE ( 'NONE', #5997, 37.50000000000000711 ) ;
#4837 = VECTOR ( 'NONE', #6802, 1000.000000000000000 ) ;
#4838 = ORIENTED_EDGE ( 'NONE', *, *, #126, .T. ) ;
#4839 = DIRECTION ( 'NONE',  ( 1.000000000000000000, 0.000000000000000000, 0.000000000000000000 ) ) ;
#4840 = ORIENTED_EDGE ( 'NONE', *, *, #2793, .F. ) ;
#4841 = FACE_BOUND ( 'NONE', #313, .T. ) ;
#4842 = ORIENTED_EDGE ( 'NONE', *, *, #2482, .F. ) ;
#4843 = CIRCLE ( 'NONE', #7161, 5.000000000000000000 ) ;
#4844 = DIRECTION ( 'NONE',  ( -0.000000000000000000, 0.000000000000000000, 1.000000000000000000 ) ) ;
#4845 = VECTOR ( 'NONE', #3223, 1000.000000000000000 ) ;
#4846 = DIRECTION ( 'NONE',  ( -0.000000000000000000, -0.000000000000000000, -1.000000000000000000 ) ) ;
#4847 = ORIENTED_EDGE ( 'NONE', *, *, #2349, .T. ) ;
#4848 = VECTOR ( 'NONE', #3924, 1000.000000000000000 ) ;
#4849 = AXIS2_PLACEMENT_3D ( 'NONE', #4767, #3661, #7311 ) ;
#4850 = VERTEX_POINT ( 'NONE', #2335 ) ;
#4851 = DIRECTION ( 'NONE',  ( -0.000000000000000000, 0.000000000000000000, 1.000000000000000000 ) ) ;
#4852 = EDGE_CURVE ( 'NONE', #556, #5242, #3578, .T. ) ;
#4853 = CARTESIAN_POINT ( 'NONE',  ( -25.00000000000000000, 0.000000000000000000, -25.00000000000000000 ) ) ;
#4854 = CARTESIAN_POINT ( 'NONE',  ( 0.000000000000000000, 0.000000000000000000, 31.24999999999999289 ) ) ;
#4855 = DIRECTION ( 'NONE',  ( 0.7071067811865482389, 0.000000000000000000, 0.7071067811865469066 ) ) ;
#4856 = CARTESIAN_POINT ( 'NONE',  ( 62.50000000000008527, 111.9999999999998863, 130.0000000000000000 ) ) ;
#4857 = CIRCLE ( 'NONE', #1397, 12.50000000000001066 ) ;
#4858 = CARTESIAN_POINT ( 'NONE',  ( 0.000000000000000000, 0.000000000000000000, 2.000000000000001776 ) ) ;
#4859 = CARTESIAN_POINT ( 'NONE',  ( 326.6025403784437913, 149.9999999999999716, 125.0000000000000000 ) ) ;
#4860 = ITEM_DEFINED_TRANSFORMATION ( 'NONE', 'NONE', #5270,  #5785 ) ;
#4861 = CARTESIAN_POINT ( 'NONE',  ( -24.28095581706361727, -30.59582894744887582, 12.50000000000000000 ) ) ;
#4862 = CARTESIAN_POINT ( 'NONE',  ( 296.6025403784437913, 142.5000000000000000, 17.49999999999998934 ) ) ;
#4863 = DIRECTION ( 'NONE',  ( 0.000000000000000000, -1.000000000000000000, 0.000000000000000000 ) ) ;
#4864 = ORIENTED_EDGE ( 'NONE', *, *, #3585, .T. ) ;
#4865 = ORIENTED_EDGE ( 'NONE', *, *, #3526, .T. ) ;
#4866 = DIRECTION ( 'NONE',  ( -0.000000000000000000, -0.000000000000000000, -1.000000000000000000 ) ) ;
#4867 = FACE_OUTER_BOUND ( 'NONE', #2661, .T. ) ;
#4868 = DIRECTION ( 'NONE',  ( 0.000000000000000000, 0.000000000000000000, -1.000000000000000000 ) ) ;
#4869 = DIRECTION ( 'NONE',  ( -0.000000000000000000, -0.000000000000000000, -1.000000000000000000 ) ) ;
#4870 = ORIENTED_EDGE ( 'NONE', *, *, #2435, .T. ) ;
#4871 = AXIS2_PLACEMENT_3D ( 'NONE', #1580, #3277, #227 ) ;
#4872 = PLANE ( 'NONE',  #6098 ) ;
#4873 = EDGE_CURVE ( 'NONE', #886, #7894, #7858, .T. ) ;
#4874 = ORIENTED_EDGE ( 'NONE', *, *, #3760, .T. ) ;
#4875 = EDGE_CURVE ( 'NONE', #4540, #2, #5583, .T. ) ;
#4876 = CARTESIAN_POINT ( 'NONE',  ( 364.1923384560104182, 18.98451973267744464, 6.332666029034883515 ) ) ;
#4877 = ORIENTED_EDGE ( 'NONE', *, *, #4427, .F. ) ;
#4878 = CARTESIAN_POINT ( 'NONE',  ( 364.8788272836525266, -18.60519396204907139, 7.346513279853128964 ) ) ;
#4879 = EDGE_LOOP ( 'NONE', ( #2898, #607, #152, #7895 ) ) ;
#4880 = LINE ( 'NONE', #6135, #2665 ) ;
#4881 = FACE_BOUND ( 'NONE', #2544, .T. ) ;
#4882 = EDGE_CURVE ( 'NONE', #646, #36, #80, .T. ) ;
#4883 = EDGE_CURVE ( 'NONE', #6898, #116, #1629, .T. ) ;
#4884 = EDGE_LOOP ( 'NONE', ( #5196, #1761, #6157, #3720, #5008 ) ) ;
#4885 = ORIENTED_EDGE ( 'NONE', *, *, #6422, .T. ) ;
#4886 = ORIENTED_EDGE ( 'NONE', *, *, #4401, .T. ) ;
#4887 = DIRECTION ( 'NONE',  ( 0.000000000000000000, 0.000000000000000000, 1.000000000000000000 ) ) ;
#4888 = CARTESIAN_POINT ( 'NONE',  ( 2.775557561562891351E-14, 262.5000000000000568, 12.50000000000000000 ) ) ;
#4889 = DIRECTION ( 'NONE',  ( 0.000000000000000000, -1.000000000000000000, 0.000000000000000000 ) ) ;
#4890 = CARTESIAN_POINT ( 'NONE',  ( 42.08354679051385006, 177.5000000000000000, 12.55124306091975761 ) ) ;
#4891 = CARTESIAN_POINT ( 'NONE',  ( 9.381941874331417353, -16.24999999999999645, 7.500000000000000000 ) ) ;
#4892 = CARTESIAN_POINT ( 'NONE',  ( 385.5807152618725127, 18.85911174686545166, -6.667915149371354211 ) ) ;
#4893 = APPLICATION_CONTEXT ( 'automotive_design' ) ;
#4894 = EDGE_CURVE ( 'NONE', #4382, #2195, #3814, .T. ) ;
#4895 = CYLINDRICAL_SURFACE ( 'NONE', #4977, 20.00000000000000000 ) ;
#4896 = ITEM_DEFINED_TRANSFORMATION ( 'NONE', 'NONE', #406,  #5785 ) ;
#4897 =( LENGTH_UNIT ( ) NAMED_UNIT ( * ) SI_UNIT ( .MILLI., .METRE. ) );
#4898 = DIRECTION ( 'NONE',  ( 0.000000000000000000, -0.000000000000000000, 1.000000000000000000 ) ) ;
#4899 = DIRECTION ( 'NONE',  ( -0.000000000000000000, -0.000000000000000000, -1.000000000000000000 ) ) ;
#4900 = CIRCLE ( 'NONE', #5150, 24.99999996734539920 ) ;
#4901 = DIRECTION ( 'NONE',  ( 1.000000000000000000, 0.000000000000000000, 0.000000000000000000 ) ) ;
#4902 = ORIENTED_EDGE ( 'NONE', *, *, #5241, .T. ) ;
#4903 = AXIS2_PLACEMENT_3D ( 'NONE', #2238, #2069, #830 ) ;
#4904 = ORIENTED_EDGE ( 'NONE', *, *, #3899, .F. ) ;
#4905 = DIRECTION ( 'NONE',  ( 1.000000000000000000, 0.000000000000000000, 0.000000000000000000 ) ) ;
#4906 = DIRECTION ( 'NONE',  ( 0.000000000000000000, 0.000000000000000000, 1.000000000000000000 ) ) ;
#4907 = CARTESIAN_POINT ( 'NONE',  ( -48.67326389759909944, 48.65950482248330644, 12.50000000000000000 ) ) ;
#4908 = SURFACE_STYLE_FILL_AREA ( #4231 ) ;
#4909 = ORIENTED_EDGE ( 'NONE', *, *, #661, .F. ) ;
#4910 = VECTOR ( 'NONE', #4131, 1000.000000000000000 ) ;
#4911 = FACE_OUTER_BOUND ( 'NONE', #7205, .T. ) ;
#4912 = VECTOR ( 'NONE', #3387, 1000.000000000000000 ) ;
#4913 = ORIENTED_EDGE ( 'NONE', *, *, #6302, .F. ) ;
#4914 = CIRCLE ( 'NONE', #182, 12.50000000000000000 ) ;
#4915 = CARTESIAN_POINT ( 'NONE',  ( 374.1490196022552936, 15.63011725355127624, 12.47807683047398619 ) ) ;
#4916 = TOROIDAL_SURFACE ( 'NONE', #7229, 15.00000000000000000, 5.000000000000000000 ) ;
#4917 = VERTEX_POINT ( 'NONE', #1288 ) ;
#4918 = CARTESIAN_POINT ( 'NONE',  ( 363.3225212018339789, -19.49607926063143282, -4.478210459206754201 ) ) ;
#4919 = ORIENTED_EDGE ( 'NONE', *, *, #5175, .T. ) ;
#4920 = EDGE_CURVE ( 'NONE', #6102, #2041, #4443, .T. ) ;
#4921 = CARTESIAN_POINT ( 'NONE',  ( -66.45428044951677293, 30.87346046883880035, 0.000000000000000000 ) ) ;
#4922 = DIRECTION ( 'NONE',  ( 1.000000000000000000, 0.000000000000000000, 0.000000000000000000 ) ) ;
#4923 = CIRCLE ( 'NONE', #4028, 12.50000000000001066 ) ;
#4924 = EDGE_CURVE ( 'NONE', #6545, #2977, #5, .T. ) ;
#4925 = CIRCLE ( 'NONE', #1467, 25.00000000000000000 ) ;
#4926 = VERTEX_POINT ( 'NONE', #1956 ) ;
#4927 = VERTEX_POINT ( 'NONE', #1362 ) ;
#4928 = AXIS2_PLACEMENT_3D ( 'NONE', #1384, #1658, #6283 ) ;
#4929 = EDGE_CURVE ( 'NONE', #1830, #4349, #5481, .T. ) ;
#4930 = ORIENTED_EDGE ( 'NONE', *, *, #4577, .F. ) ;
#4931 = CARTESIAN_POINT ( 'NONE',  ( -27.49999999999994671, 42.50000000000009237, 12.50000000000000000 ) ) ;
#4932 = CARTESIAN_POINT ( 'NONE',  ( 387.1681567566444642, -19.79418587323000267, 2.891333466711802469 ) ) ;
#4933 = CARTESIAN_POINT ( 'NONE',  ( 6.495190528383280260, 16.25000000000000000, 0.000000000000000000 ) ) ;
#4934 = DIRECTION ( 'NONE',  ( -1.000000000000000000, 0.000000000000000000, 0.000000000000000000 ) ) ;
#4935 = FACE_OUTER_BOUND ( 'NONE', #5274, .T. ) ;
#4936 = AXIS2_PLACEMENT_3D ( 'NONE', #2560, #4431, #2030 ) ;
#4937 = CONTEXT_DEPENDENT_SHAPE_REPRESENTATION ( #4026, #5195 ) ;
#4938 = DIRECTION ( 'NONE',  ( 0.000000000000000000, 0.000000000000000000, -1.000000000000000000 ) ) ;
#4939 = DIRECTION ( 'NONE',  ( 1.000000000000000000, -1.387778780781445676E-15, 0.000000000000000000 ) ) ;
#4941 = DIRECTION ( 'NONE',  ( 1.000000000000000000, 0.000000000000000000, 0.000000000000000000 ) ) ;
#4940 = AXIS2_PLACEMENT_3D ( 'NONE', #7687, #4307, #6716 ) ;
#4942 = FACE_OUTER_BOUND ( 'NONE', #6025, .T. ) ;
#4943 = APPLICATION_CONTEXT ( 'automotive_design' ) ;
#4944 = VERTEX_POINT ( 'NONE', #6145 ) ;
#4945 = SHAPE_REPRESENTATION_RELATIONSHIP ( 'NONE' , 'NONE' ,  #949, #1434 ) ;
#4946 = ORIENTED_EDGE ( 'NONE', *, *, #5158, .T. ) ;
#4947 = CARTESIAN_POINT ( 'NONE',  ( 150.0000000000000000, 1.836970198721029747E-14, 25.00000000000000000 ) ) ;
#4948 = CARTESIAN_POINT ( 'NONE',  ( 362.5000000000001137, -4.592425496802566478E-15, 25.00000000000000000 ) ) ;
#4949 = CARTESIAN_POINT ( 'NONE',  ( 0.000000000000000000, -25.00000000000000000, 25.00000000000000000 ) ) ;
#4950 = EDGE_CURVE ( 'NONE', #279, #1497, #649, .T. ) ;
#4951 = CARTESIAN_POINT ( 'NONE',  ( 12.50000000000000000, 1.530808498934191521E-15, 25.00000000000000000 ) ) ;
#4952 = ORIENTED_EDGE ( 'NONE', *, *, #4738, .T. ) ;
#4953 = AXIS2_PLACEMENT_3D ( 'NONE', #1338, #4420, #6801 ) ;
#4954 = CARTESIAN_POINT ( 'NONE',  ( 314.1025403784437913, 150.0000000000000568, 125.0000000000000000 ) ) ;
#4955 = ORIENTED_EDGE ( 'NONE', *, *, #3676, .T. ) ;
#4956 = AXIS2_PLACEMENT_3D ( 'NONE', #3713, #3222, #7397 ) ;
#4957 = CARTESIAN_POINT ( 'NONE',  ( 367.6909075080810112, 17.23604965026853009, 10.14822696828370319 ) ) ;
#4958 = ORIENTED_EDGE ( 'NONE', *, *, #6771, .F. ) ;
#4959 = DIRECTION ( 'NONE',  ( 1.000000000000000000, -0.000000000000000000, 0.000000000000000000 ) ) ;
#4960 = ORIENTED_EDGE ( 'NONE', *, *, #3760, .F. ) ;
#4961 = SURFACE_SIDE_STYLE ('',( #4280 ) ) ;
#4962 = DIRECTION ( 'NONE',  ( -1.000000000000000000, 0.000000000000000000, 0.000000000000000000 ) ) ;
#4963 = AXIS2_PLACEMENT_3D ( 'NONE', #3249, #3970, #2121 ) ;
#4964 = VECTOR ( 'NONE', #2080, 1000.000000000000000 ) ;
#4965 = EDGE_LOOP ( 'NONE', ( #2258, #2361, #7386, #6412 ) ) ;
#4966 = EDGE_CURVE ( 'NONE', #905, #2348, #5045, .T. ) ;
#4967 = ORIENTED_EDGE ( 'NONE', *, *, #3125, .F. ) ;
#4968 = AXIS2_PLACEMENT_3D ( 'NONE', #153, #1991, #4515 ) ;
#4969 = AXIS2_PLACEMENT_3D ( 'NONE', #3085, #1269, #3117 ) ;
#4970 = EDGE_LOOP ( 'NONE', ( #4885, #3528, #6453, #18 ) ) ;
#4971 = EDGE_CURVE ( 'NONE', #4547, #4474, #7901, .T. ) ;
#4972 = DIRECTION ( 'NONE',  ( 0.000000000000000000, 0.000000000000000000, 1.000000000000000000 ) ) ;
#4973 = CARTESIAN_POINT ( 'NONE',  ( 382.6434889735085108, -17.37246880845878039, -9.923319895790875478 ) ) ;
#4974 = DIRECTION ( 'NONE',  ( 0.000000000000000000, 0.000000000000000000, -1.000000000000000000 ) ) ;
#4975 = CARTESIAN_POINT ( 'NONE',  ( -31.24999999999997158, 79.24999999999992895, 130.0000000000000000 ) ) ;
#4976 = CARTESIAN_POINT ( 'NONE',  ( 0.000000000000000000, 0.000000000000000000, 25.00000000000000000 ) ) ;
#4977 = AXIS2_PLACEMENT_3D ( 'NONE', #6671, #7352, #2039 ) ;
#4978 = AXIS2_PLACEMENT_3D ( 'NONE', #5168, #7586, #4496 ) ;
#4979 = ADVANCED_BREP_SHAPE_REPRESENTATION ( '', ( #1475, #5785 ), #1293 ) ;
#4980 = EDGE_CURVE ( 'NONE', #3684, #3773, #4568, .T. ) ;
#4981 = EDGE_CURVE ( 'NONE', #7631, #103, #7267, .T. ) ;
#4982 = SHAPE_DEFINITION_REPRESENTATION ( #3283, #6180 ) ;
#4983 = AXIS2_PLACEMENT_3D ( 'NONE', #2324, #4758, #7217 ) ;
#4984 = CARTESIAN_POINT ( 'NONE',  ( 296.6025403784439050, 87.50000000000005684, 17.49999999999998934 ) ) ;
#4985 = CARTESIAN_POINT ( 'NONE',  ( 4.000000000000004441, 0.000000000000000000, 0.000000000000000000 ) ) ;
#4986 = CIRCLE ( 'NONE', #7807, 12.50000000000001066 ) ;
#4987 = FACE_OUTER_BOUND ( 'NONE', #7307, .T. ) ;
#4988 = CARTESIAN_POINT ( 'NONE',  ( -26.24999999999997158, 0.000000000000000000, 12.50000000000000000 ) ) ;
#4989 = EDGE_CURVE ( 'NONE', #28, #4723, #736, .T. ) ;
#4990 = EDGE_CURVE ( 'NONE', #7303, #7839, #4320, .T. ) ;
#4991 = ORIENTED_EDGE ( 'NONE', *, *, #5214, .F. ) ;
#4992 = ORIENTED_EDGE ( 'NONE', *, *, #2078, .F. ) ;
#4993 = DIRECTION ( 'NONE',  ( 0.000000000000000000, 0.000000000000000000, 1.000000000000000000 ) ) ;
#4994 = CARTESIAN_POINT ( 'NONE',  ( -74.28095588234631919, 0.000000000000000000, 12.50000000000000000 ) ) ;
#4995 = CARTESIAN_POINT ( 'NONE',  ( -12.50000000000000000, 0.000000000000000000, 7.500000000000000000 ) ) ;
#4996 = CARTESIAN_POINT ( 'NONE',  ( 25.00000000000000000, -25.00000000000000000, 0.000000000000000000 ) ) ;
#4997 = VERTEX_POINT ( 'NONE', #3063 ) ;
#4998 = DIRECTION ( 'NONE',  ( 0.8948607650084221543, -4.286094916964204981E-16, 0.4463453945640545317 ) ) ;
#4999 = EDGE_CURVE ( 'NONE', #5569, #5360, #4190, .T. ) ;
#5000 = CARTESIAN_POINT ( 'NONE',  ( 362.8318432433553085, 19.79418587323000267, 2.891333466711802469 ) ) ;
#5001 = VERTEX_POINT ( 'NONE', #6820 ) ;
#5002 = CARTESIAN_POINT ( 'NONE',  ( 46.25000000000002842, 177.5000000000000000, 195.5000000000000000 ) ) ;
#5003 = ORIENTED_EDGE ( 'NONE', *, *, #3416, .F. ) ;
#5004 = FACE_BOUND ( 'NONE', #230, .T. ) ;
#5005 = DIRECTION ( 'NONE',  ( -0.000000000000000000, -0.000000000000000000, -1.000000000000000000 ) ) ;
#5006 = VERTEX_POINT ( 'NONE', #2528 ) ;
#5007 = VERTEX_POINT ( 'NONE', #1840 ) ;
#5008 = ORIENTED_EDGE ( 'NONE', *, *, #1504, .F. ) ;
#5009 = LINE ( 'NONE', #7462, #5999 ) ;
#5010 = CARTESIAN_POINT ( 'NONE',  ( -31.24999999999997158, 177.4999999999999432, 195.5000000000000000 ) ) ;
#5011 = CYLINDRICAL_SURFACE ( 'NONE', #5013, 25.00000000000000000 ) ;
#5012 = VERTEX_POINT ( 'NONE', #5459 ) ;
#5013 = AXIS2_PLACEMENT_3D ( 'NONE', #6064, #7898, #3104 ) ;
#5014 = DIRECTION ( 'NONE',  ( 1.000000000000000000, 0.000000000000000000, 0.000000000000000000 ) ) ;
#5015 = DIRECTION ( 'NONE',  ( -0.000000000000000000, -0.000000000000000000, -1.000000000000000000 ) ) ;
#5016 = CARTESIAN_POINT ( 'NONE',  ( -9.381941874331412023, -16.24999999999999645, 7.500000000000000000 ) ) ;
#5017 = DIRECTION ( 'NONE',  ( -0.000000000000000000, -0.000000000000000000, -1.000000000000000000 ) ) ;
#5018 = CARTESIAN_POINT ( 'NONE',  ( 190.0000000000000000, 0.000000000000000000, 0.000000000000000000 ) ) ;
#5019 = ADVANCED_FACE ( 'NONE', ( #2452, #7387 ), #1882, .F. ) ;
#5020 = EDGE_CURVE ( 'NONE', #7081, #5902, #4289, .T. ) ;
#5021 = ORIENTED_EDGE ( 'NONE', *, *, #1154, .T. ) ;
#5022 =( NAMED_UNIT ( * ) SI_UNIT ( $, .STERADIAN. ) SOLID_ANGLE_UNIT ( ) );
#5023 = ORIENTED_EDGE ( 'NONE', *, *, #190, .F. ) ;
#5024 = CYLINDRICAL_SURFACE ( 'NONE', #1896, 5.000000000000004441 ) ;
#5025 = LINE ( 'NONE', #7367, #6585 ) ;
#5026 = EDGE_CURVE ( 'NONE', #869, #2966, #1321, .T. ) ;
#5027 = LINE ( 'NONE', #7481, #951 ) ;
#5028 = ORIENTED_EDGE ( 'NONE', *, *, #7514, .F. ) ;
#5029 = FACE_OUTER_BOUND ( 'NONE', #2298, .T. ) ;
#5030 = CARTESIAN_POINT ( 'NONE',  ( 362.6662177141545271, 19.89643035834168927, 2.074044983930025232 ) ) ;
#5031 = ORIENTED_EDGE ( 'NONE', *, *, #718, .T. ) ;
#5032 = CARTESIAN_POINT ( 'NONE',  ( -12.50000000000000355, 1.530808498934191916E-15, 77.49999999999998579 ) ) ;
#5033 = ORIENTED_EDGE ( 'NONE', *, *, #3496, .T. ) ;
#5034 = VECTOR ( 'NONE', #2120, 1000.000000000000000 ) ;
#5035 = CARTESIAN_POINT ( 'NONE',  ( -12.50000000000000000, -25.00000000000000355, 37.50000000000000000 ) ) ;
#5036 = LINE ( 'NONE', #4435, #3523 ) ;
#5037 = EDGE_CURVE ( 'NONE', #6276, #2643, #3434, .T. ) ;
#5038 = AXIS2_PLACEMENT_3D ( 'NONE', #850, #2822, #7588 ) ;
#5039 = ORIENTED_EDGE ( 'NONE', *, *, #2721, .T. ) ;
#5040 = CIRCLE ( 'NONE', #1452, 12.50000000000001776 ) ;
#5041 = FACE_OUTER_BOUND ( 'NONE', #839, .T. ) ;
#5042 = VERTEX_POINT ( 'NONE', #6740 ) ;
#5043 = ORIENTED_EDGE ( 'NONE', *, *, #504, .F. ) ;
#5044 = DIRECTION ( 'NONE',  ( -0.000000000000000000, -0.000000000000000000, -1.000000000000000000 ) ) ;
#5045 = LINE ( 'NONE', #5010, #2408 ) ;
#5046 = ORIENTED_EDGE ( 'NONE', *, *, #1501, .F. ) ;
#5047 = CIRCLE ( 'NONE', #4273, 31.78244274809162562 ) ;
#5048 = AXIS2_PLACEMENT_3D ( 'NONE', #3432, #2185, #4022 ) ;
#5049 = DIRECTION ( 'NONE',  ( 4.789677997474698199E-16, -1.000000000000000000, 0.000000000000000000 ) ) ;
#5050 = ADVANCED_FACE ( 'NONE', ( #5413 ), #6699, .T. ) ;
#5051 = AXIS2_PLACEMENT_3D ( 'NONE', #7400, #6272, #4373 ) ;
#5052 = DIRECTION ( 'NONE',  ( 0.000000000000000000, 1.000000000000000000, 0.000000000000000000 ) ) ;
#5053 = DIRECTION ( 'NONE',  ( 1.000000000000000000, 0.000000000000000000, 0.000000000000000000 ) ) ;
#5054 = CARTESIAN_POINT ( 'NONE',  ( 72.36967921662629522, 50.20544122544588816, 12.50000000000000000 ) ) ;
#5055 = CARTESIAN_POINT ( 'NONE',  ( 286.6025403784439050, 90.00000000000001421, 0.000000000000000000 ) ) ;
#5056 = ADVANCED_FACE ( 'NONE', ( #648 ), #2490, .F. ) ;
#5057 = ORIENTED_EDGE ( 'NONE', *, *, #7686, .F. ) ;
#5058 = CYLINDRICAL_SURFACE ( 'NONE', #2299, 5.000000000000000888 ) ;
#5059 = ADVANCED_FACE ( 'NONE', ( #5699 ), #5156, .T. ) ;
#5060 = VECTOR ( 'NONE', #2403, 1000.000000000000000 ) ;
#5061 = DIRECTION ( 'NONE',  ( 1.000000000000000000, 0.000000000000000000, 0.000000000000000000 ) ) ;
#5062 = ORIENTED_EDGE ( 'NONE', *, *, #6562, .T. ) ;
#5063 = CARTESIAN_POINT ( 'NONE',  ( 190.0000000000000000, 0.000000000000000000, 15.00000000000000000 ) ) ;
#5064 = CARTESIAN_POINT ( 'NONE',  ( 12.50000000000000000, 1.530808498934191127E-15, 90.00000000000000000 ) ) ;
#5065 = FACE_OUTER_BOUND ( 'NONE', #5684, .T. ) ;
#5066 = EDGE_CURVE ( 'NONE', #4500, #5961, #3290, .T. ) ;
#5067 = LINE ( 'NONE', #859, #1719 ) ;
#5068 = VERTEX_POINT ( 'NONE', #762 ) ;
#5069 = EDGE_CURVE ( 'NONE', #6800, #4076, #3302, .T. ) ;
#5070 = EDGE_LOOP ( 'NONE', ( #1797, #1427 ) ) ;
#5071 = EDGE_CURVE ( 'NONE', #3842, #1519, #92, .T. ) ;
#5072 = CARTESIAN_POINT ( 'NONE',  ( 37.50000000000000711, 42.50000000000003553, 0.000000000000000000 ) ) ;
#5073 = ORIENTED_EDGE ( 'NONE', *, *, #6118, .T. ) ;
#5074 = CYLINDRICAL_SURFACE ( 'NONE', #1098, 12.50000000000000000 ) ;
#5075 = CIRCLE ( 'NONE', #2654, 12.50000000000001066 ) ;
#5076 = EDGE_LOOP ( 'NONE', ( #2277, #4153, #7731, #7576 ) ) ;
#5077 = CARTESIAN_POINT ( 'NONE',  ( 25.71904415029483459, 19.40417101989674009, 12.50000000000000000 ) ) ;
#5078 = CYLINDRICAL_SURFACE ( 'NONE', #4408, 25.00000000000000000 ) ;
#5079 = ADVANCED_FACE ( 'NONE', ( #4563 ), #7524, .T. ) ;
#5080 = VECTOR ( 'NONE', #4731, 1000.000000000000000 ) ;
#5081 = VERTEX_POINT ( 'NONE', #6374 ) ;
#5082 = CARTESIAN_POINT ( 'NONE',  ( 339.1025403784438481, 150.0000000000000568, 125.0000000000000000 ) ) ;
#5083 = EDGE_LOOP ( 'NONE', ( #515, #5046, #761, #3574 ) ) ;
#5084 = ORIENTED_EDGE ( 'NONE', *, *, #4211, .T. ) ;
#5085 = CARTESIAN_POINT ( 'NONE',  ( 12.50000000000000355, 0.000000000000000000, 92.50000000000000000 ) ) ;
#5086 = DIRECTION ( 'NONE',  ( -0.000000000000000000, -0.000000000000000000, 1.000000000000000000 ) ) ;
#5087 = DIRECTION ( 'NONE',  ( 0.000000000000000000, 0.000000000000000000, -1.000000000000000000 ) ) ;
#5089 = ORIENTED_EDGE ( 'NONE', *, *, #3726, .F. ) ;
#5088 = CONICAL_SURFACE ( 'NONE', #5207, 18.75000000000009948, 0.7853981633974421728 ) ;
#5090 = CYLINDRICAL_SURFACE ( 'NONE', #6329, 5.000000000000004441 ) ;
#5091 = AXIS2_PLACEMENT_3D ( 'NONE', #361, #3411, #1642 ) ;
#5092 = VECTOR ( 'NONE', #1736, 1000.000000000000000 ) ;
#5093 = EDGE_CURVE ( 'NONE', #4679, #2900, #3247, .T. ) ;
#5094 = DIRECTION ( 'NONE',  ( -1.000000000000000000, 0.000000000000000000, 0.000000000000000000 ) ) ;
#5095 = CARTESIAN_POINT ( 'NONE',  ( 0.000000000000000000, 0.000000000000000000, 6.999999999999999112 ) ) ;
#5096 = CYLINDRICAL_SURFACE ( 'NONE', #4406, 12.50000000000001066 ) ;
#5097 = CARTESIAN_POINT ( 'NONE',  ( 412.4999999999998863, 142.5000000000000000, 17.49999999999998934 ) ) ;
#5098 = TOROIDAL_SURFACE ( 'NONE', #1647, 12.50000000000000355, 5.000000000000000000 ) ;
#5099 = VECTOR ( 'NONE', #13, 1000.000000000000000 ) ;
#5100 = ORIENTED_EDGE ( 'NONE', *, *, #5326, .T. ) ;
#5101 = CIRCLE ( 'NONE', #6140, 25.00000003264134918 ) ;
#5102 = VECTOR ( 'NONE', #6384, 1000.000000000000114 ) ;
#5103 = DIRECTION ( 'NONE',  ( 1.000000000000000000, 0.000000000000000000, 0.000000000000000000 ) ) ;
#5104 = ORIENTED_EDGE ( 'NONE', *, *, #864, .T. ) ;
#5105 = DIRECTION ( 'NONE',  ( -1.000000000000000000, -0.000000000000000000, 0.000000000000000000 ) ) ;
#5106 = DIRECTION ( 'NONE',  ( -0.000000000000000000, -0.000000000000000000, -1.000000000000000000 ) ) ;
#5107 = CARTESIAN_POINT ( 'NONE',  ( 412.5000000000000000, 87.50000000000005684, 12.50000000000000000 ) ) ;
#5108 = DIRECTION ( 'NONE',  ( -0.000000000000000000, 0.000000000000000000, 1.000000000000000000 ) ) ;
#5109 = ORIENTED_EDGE ( 'NONE', *, *, #1644, .F. ) ;
#5110 = PRODUCT_DEFINITION_CONTEXT ( 'detailed design', #694, 'design' ) ;
#5111 = CARTESIAN_POINT ( 'NONE',  ( 314.1025403784437913, 150.0000000000000568, 125.0000000000000000 ) ) ;
#5112 = ORIENTED_EDGE ( 'NONE', *, *, #3995, .F. ) ;
#5113 = CARTESIAN_POINT ( 'NONE',  ( -12.50000000000000355, 1.836970198721030378E-15, 82.49999999999998579 ) ) ;
#5114 = DIRECTION ( 'NONE',  ( -1.000000000000000000, 0.000000000000000000, 0.000000000000000000 ) ) ;
#5115 = DIRECTION ( 'NONE',  ( 0.000000000000000000, 0.000000000000000000, 1.000000000000000000 ) ) ;
#5116 = CARTESIAN_POINT ( 'NONE',  ( -25.00000000000000711, 0.000000000000000000, 25.00000000000000000 ) ) ;
#5117 = EDGE_CURVE ( 'NONE', #1320, #7097, #3177, .T. ) ;
#5118 = EDGE_CURVE ( 'NONE', #260, #6817, #5861, .T. ) ;
#5119 = VERTEX_POINT ( 'NONE', #1955 ) ;
#5120 = DIRECTION ( 'NONE',  ( -0.9335804380297003657, 0.3583679195021128305, 0.000000000000000000 ) ) ;
#5121 = ORIENTED_EDGE ( 'NONE', *, *, #1111, .T. ) ;
#5122 = ORIENTED_EDGE ( 'NONE', *, *, #2623, .F. ) ;
#5123 = DIRECTION ( 'NONE',  ( -1.000000000000000000, 1.224646799147353454E-16, 0.000000000000000000 ) ) ;
#5124 = SURFACE_SIDE_STYLE ('',( #4524 ) ) ;
#5125 = CARTESIAN_POINT ( 'NONE',  ( 175.0000000000000000, 0.000000000000000000, 0.000000000000000000 ) ) ;
#5126 =( GEOMETRIC_REPRESENTATION_CONTEXT ( 3 ) GLOBAL_UNCERTAINTY_ASSIGNED_CONTEXT ( ( #2556 ) ) GLOBAL_UNIT_ASSIGNED_CONTEXT ( ( #2962, #1626, #2318 ) ) REPRESENTATION_CONTEXT ( 'NONE', 'WORKASPACE' ) );
#5127 = ORIENTED_EDGE ( 'NONE', *, *, #2053, .T. ) ;
#5128 = PRODUCT_DEFINITION_FORMATION_WITH_SPECIFIED_SOURCE ( 'ANY', '', #2198, .NOT_KNOWN. ) ;
#5129 = CARTESIAN_POINT ( 'NONE',  ( 337.5000000000000568, -6.123233995736758985E-15, 25.00000000000000000 ) ) ;
#5130 = DIRECTION ( 'NONE',  ( 1.000000000000000000, 0.000000000000000000, 0.000000000000000000 ) ) ;
#5131 = CARTESIAN_POINT ( 'NONE',  ( 137.4999999999999716, 1.836970198721029747E-14, 25.00000000000000000 ) ) ;
#5132 = DIRECTION ( 'NONE',  ( 0.000000000000000000, 0.000000000000000000, 1.000000000000000000 ) ) ;
#5133 = EDGE_CURVE ( 'NONE', #7097, #4609, #1120, .T. ) ;
#5134 = ORIENTED_EDGE ( 'NONE', *, *, #1177, .T. ) ;
#5135 = CARTESIAN_POINT ( 'NONE',  ( -16.96112411586215529, 80.38061160285559481, 12.50000000000000000 ) ) ;
#5136 = EDGE_LOOP ( 'NONE', ( #6139, #3694, #2701, #2451 ) ) ;
#5137 = DIRECTION ( 'NONE',  ( 0.000000000000000000, -1.387778780781445676E-16, 1.000000000000000000 ) ) ;
#5138 = DIRECTION ( 'NONE',  ( 0.000000000000000000, 0.000000000000000000, -1.000000000000000000 ) ) ;
#5139 = LINE ( 'NONE', #2626, #2611 ) ;
#5140 = DIRECTION ( 'NONE',  ( -1.000000000000000000, 4.270088556250607616E-16, -0.000000000000000000 ) ) ;
#5141 = ORIENTED_EDGE ( 'NONE', *, *, #7166, .F. ) ;
#5142 = VERTEX_POINT ( 'NONE', #2726 ) ;
#5143 = FACE_OUTER_BOUND ( 'NONE', #4621, .T. ) ;
#5144 = VERTEX_POINT ( 'NONE', #121 ) ;
#5145 = CARTESIAN_POINT ( 'NONE',  ( -32.49999999999997158, 1.387778780781446307E-14, 5.000000000000000000 ) ) ;
#5146 = FACE_OUTER_BOUND ( 'NONE', #35, .T. ) ;
#5147 = EDGE_CURVE ( 'NONE', #443, #7839, #5608, .T. ) ;
#5148 = LINE ( 'NONE', #5035, #5874 ) ;
#5149 = DIRECTION ( 'NONE',  ( -1.000000000000000000, -0.000000000000000000, -0.000000000000000000 ) ) ;
#5150 = AXIS2_PLACEMENT_3D ( 'NONE', #3886, #882, #5202 ) ;
#5151 = ORIENTED_EDGE ( 'NONE', *, *, #2407, .T. ) ;
#5152 = DIRECTION ( 'NONE',  ( 1.000000000000000000, -0.000000000000000000, -0.000000000000000000 ) ) ;
#5153 = ORIENTED_EDGE ( 'NONE', *, *, #1303, .T. ) ;
#5154 = EDGE_CURVE ( 'NONE', #5578, #4446, #7542, .T. ) ;
#5155 = ORIENTED_EDGE ( 'NONE', *, *, #1226, .F. ) ;
#5156 = PLANE ( 'NONE',  #3056 ) ;
#5157 = CARTESIAN_POINT ( 'NONE',  ( 25.00000000000000000, 1.530808498934191521E-15, 12.50000000000000000 ) ) ;
#5158 = EDGE_CURVE ( 'NONE', #1115, #4430, #4445, .T. ) ;
#5159 = DIRECTION ( 'NONE',  ( 1.000000000000000000, 0.000000000000000000, 0.000000000000000000 ) ) ;
#5160 = CIRCLE ( 'NONE', #5694, 18.75000000000009948 ) ;
#5161 = EDGE_CURVE ( 'NONE', #443, #6889, #6863, .T. ) ;
#5162 = ORIENTED_EDGE ( 'NONE', *, *, #5475, .T. ) ;
#5163 = EDGE_CURVE ( 'NONE', #477, #3284, #1373, .T. ) ;
#5164 = VECTOR ( 'NONE', #5663, 1000.000000000000000 ) ;
#5165 = ITEM_DEFINED_TRANSFORMATION ( 'NONE', 'NONE', #659,  #5785 ) ;
#5166 = AXIS2_PLACEMENT_3D ( 'NONE', #1906, #818, #705 ) ;
#5167 = DIRECTION ( 'NONE',  ( 1.000000000000000000, 0.000000000000000000, 0.000000000000000000 ) ) ;
#5168 = CARTESIAN_POINT ( 'NONE',  ( -12.99038105676657651, 1.734723475976807094E-15, 0.000000000000000000 ) ) ;
#5169 = LINE ( 'NONE', #5054, #3016 ) ;
#5170 = DIRECTION ( 'NONE',  ( 0.000000000000000000, 0.000000000000000000, 1.000000000000000000 ) ) ;
#5171 = DIRECTION ( 'NONE',  ( 1.000000000000000000, -0.000000000000000000, 0.000000000000000000 ) ) ;
#5172 = VECTOR ( 'NONE', #1552, 1000.000000000000000 ) ;
#5173 = AXIS2_PLACEMENT_3D ( 'NONE', #7511, #6345, #3753 ) ;
#5174 = CIRCLE ( 'NONE', #1602, 4.999999999999997335 ) ;
#5175 = EDGE_CURVE ( 'NONE', #2269, #4603, #6260, .T. ) ;
#5176 = CARTESIAN_POINT ( 'NONE',  ( 399.3518360003419048, -12.50000000000000000, -13.85262921941843750 ) ) ;
#5177 = DIRECTION ( 'NONE',  ( 1.000000000000000000, 0.000000000000000000, 0.000000000000000000 ) ) ;
#5178 = VERTEX_POINT ( 'NONE', #6222 ) ;
#5179 = DIRECTION ( 'NONE',  ( -0.000000000000000000, -0.000000000000000000, -1.000000000000000000 ) ) ;
#5180 = DIRECTION ( 'NONE',  ( -0.000000000000000000, -0.000000000000000000, -1.000000000000000000 ) ) ;
#5182 = CARTESIAN_POINT ( 'NONE',  ( 50.71904415029504065, 62.70544120911855401, 12.50000000000000000 ) ) ;
#5181 = AXIS2_PLACEMENT_3D ( 'NONE', #1345, #3798, #636 ) ;
#5183 = FACE_BOUND ( 'NONE', #6930, .T. ) ;
#5184 = EDGE_LOOP ( 'NONE', ( #7218, #7087, #3403, #7299 ) ) ;
#5185 = EDGE_CURVE ( 'NONE', #6592, #2505, #5009, .T. ) ;
#5186 = EDGE_LOOP ( 'NONE', ( #5304, #7685, #7172, #4268 ) ) ;
#5187 = CARTESIAN_POINT ( 'NONE',  ( 326.6025403784438481, 142.5000000000000000, 125.0000000000000000 ) ) ;
#5188 = ORIENTED_EDGE ( 'NONE', *, *, #4428, .T. ) ;
#5189 = ADVANCED_FACE ( 'NONE', ( #3214 ), #159, .F. ) ;
#5190 = DIRECTION ( 'NONE',  ( 0.000000000000000000, 0.000000000000000000, 1.000000000000000000 ) ) ;
#5191 = CARTESIAN_POINT ( 'NONE',  ( 190.0000000000000000, 0.000000000000000000, 0.000000000000000000 ) ) ;
#5192 = SURFACE_STYLE_FILL_AREA ( #3445 ) ;
#5193 = CIRCLE ( 'NONE', #4303, 5.000000000000004441 ) ;
#5194 = CARTESIAN_POINT ( 'NONE',  ( 337.5000000000000568, -6.123233995736758985E-15, 0.000000000000000000 ) ) ;
#5195 = PRODUCT_DEFINITION_SHAPE ( 'NONE', 'NONE',  #7924 ) ;
#5196 = ORIENTED_EDGE ( 'NONE', *, *, #6570, .F. ) ;
#5197 = CARTESIAN_POINT ( 'NONE',  ( 75.00000000000000000, 10.56842436860067735, 0.000000000000000000 ) ) ;
#5198 = ORIENTED_EDGE ( 'NONE', *, *, #5514, .T. ) ;
#5199 = CARTESIAN_POINT ( 'NONE',  ( 175.0000000000000000, 1.836970198721029589E-15, -15.00000000000000000 ) ) ;
#5200 = VERTEX_POINT ( 'NONE', #6904 ) ;
#5201 = DIRECTION ( 'NONE',  ( -0.000000000000000000, 0.000000000000000000, 1.000000000000000000 ) ) ;
#5202 = DIRECTION ( 'NONE',  ( 1.000000000000000000, 0.000000000000000000, 0.000000000000000000 ) ) ;
#5203 = CARTESIAN_POINT ( 'NONE',  ( 296.6025403784437913, 149.9999999999999716, 5.000000000000000000 ) ) ;
#5204 = CARTESIAN_POINT ( 'NONE',  ( 0.000000000000000000, 0.000000000000000000, 0.000000000000000000 ) ) ;
#5205 = TOROIDAL_SURFACE ( 'NONE', #6758, 12.50000000000000355, 5.000000000000000000 ) ;
#5206 = ORIENTED_EDGE ( 'NONE', *, *, #6348, .F. ) ;
#5207 = AXIS2_PLACEMENT_3D ( 'NONE', #1185, #4604, #7653 ) ;
#5208 = CYLINDRICAL_SURFACE ( 'NONE', #3690, 25.00000003264134918 ) ;
#5209 = CARTESIAN_POINT ( 'NONE',  ( 0.000000000000000000, 0.000000000000000000, 2.500000000000085265 ) ) ;
#5210 = DIRECTION ( 'NONE',  ( 1.000000000000000000, 0.000000000000000000, 0.000000000000000000 ) ) ;
#5211 = DIRECTION ( 'NONE',  ( -4.605077885019035080E-16, -1.000000000000000000, 0.000000000000000000 ) ) ;
#5212 = DIRECTION ( 'NONE',  ( -1.000000000000000000, -0.000000000000000000, -0.000000000000000000 ) ) ;
#5213 = AXIS2_PLACEMENT_3D ( 'NONE', #4087, #3095, #4242 ) ;
#5214 = EDGE_CURVE ( 'NONE', #4671, #2998, #552, .T. ) ;
#5215 = CIRCLE ( 'NONE', #503, 13.00000000000000178 ) ;
#5216 = ADVANCED_FACE ( 'NONE', ( #1749 ), #5088, .T. ) ;
#5217 = DIRECTION ( 'NONE',  ( 1.000000000000000000, 0.000000000000000000, 0.000000000000000000 ) ) ;
#5218 = SHAPE_REPRESENTATION_RELATIONSHIP ( 'NONE' , 'NONE' ,  #7467, #4979 ) ;
#5219 = ORIENTED_EDGE ( 'NONE', *, *, #6253, .T. ) ;
#5220 = MECHANICAL_DESIGN_GEOMETRIC_PRESENTATION_REPRESENTATION (  '', ( #7660 ), #2672 ) ;
#5221 = LINE ( 'NONE', #7118, #7778 ) ;
#5222 = LINE ( 'NONE', #5064, #2295 ) ;
#5223 = CIRCLE ( 'NONE', #4583, 20.00000000000000000 ) ;
#5224 = FACE_OUTER_BOUND ( 'NONE', #1072, .T. ) ;
#5225 = PLANE ( 'NONE',  #3779 ) ;
#5226 = ORIENTED_EDGE ( 'NONE', *, *, #6651, .T. ) ;
#5227 = EDGE_CURVE ( 'NONE', #4036, #3284, #919, .T. ) ;
#5228 = AXIS2_PLACEMENT_3D ( 'NONE', #7072, #7757, #2266 ) ;
#5229 = ORIENTED_EDGE ( 'NONE', *, *, #7682, .F. ) ;
#5230 = CIRCLE ( 'NONE', #2682, 35.78244274809159720 ) ;
#5231 = EDGE_LOOP ( 'NONE', ( #4904, #4631 ) ) ;
#5232 = CARTESIAN_POINT ( 'NONE',  ( 125.0000000000000000, 0.000000000000000000, 31.25000000000000000 ) ) ;
#5233 = EDGE_LOOP ( 'NONE', ( #6319, #7723, #1511, #343, #5428, #2840, #53, #1794 ) ) ;
#5234 = DIRECTION ( 'NONE',  ( 1.000000000000000000, 0.000000000000000000, 0.000000000000000000 ) ) ;
#5235 = CARTESIAN_POINT ( 'NONE',  ( 25.00000000000000000, 24.99999999999999289, 50.00000000000000000 ) ) ;
#5236 = AXIS2_PLACEMENT_3D ( 'NONE', #4274, #1350, #3766 ) ;
#5237 = VERTEX_POINT ( 'NONE', #2769 ) ;
#5238 = FACE_BOUND ( 'NONE', #4288, .T. ) ;
#5239 =( GEOMETRIC_REPRESENTATION_CONTEXT ( 3 ) GLOBAL_UNCERTAINTY_ASSIGNED_CONTEXT ( ( #7372 ) ) GLOBAL_UNIT_ASSIGNED_CONTEXT ( ( #2445, #7379, #1316 ) ) REPRESENTATION_CONTEXT ( 'NONE', 'WORKASPACE' ) );
#5240 = DIRECTION ( 'NONE',  ( 1.000000000000000000, -4.789677997474686366E-16, 0.000000000000000000 ) ) ;
#5241 = EDGE_CURVE ( 'NONE', #3351, #4784, #6045, .T. ) ;
#5242 = VERTEX_POINT ( 'NONE', #3368 ) ;
#5243 = CARTESIAN_POINT ( 'NONE',  ( -25.00000000000000000, -25.00000000000000000, 0.000000000000000000 ) ) ;
#5244 = VERTEX_POINT ( 'NONE', #4229 ) ;
#5245 = FACE_OUTER_BOUND ( 'NONE', #3497, .T. ) ;
#5246 = EDGE_LOOP ( 'NONE', ( #7460, #434, #6314, #565 ) ) ;
#5247 = DIRECTION ( 'NONE',  ( -0.000000000000000000, 0.000000000000000000, -1.000000000000000000 ) ) ;
#5248 = DIRECTION ( 'NONE',  ( -4.789677997474686366E-16, -1.000000000000000000, -0.000000000000000000 ) ) ;
#5249 = CARTESIAN_POINT ( 'NONE',  ( -12.50000000000000000, 0.000000000000000000, 2.000000000000001776 ) ) ;
#5250 = DIRECTION ( 'NONE',  ( -0.000000000000000000, -0.000000000000000000, -1.000000000000000000 ) ) ;
#5251 = VERTEX_POINT ( 'NONE', #358 ) ;
#5252 = DIRECTION ( 'NONE',  ( 0.000000000000000000, 0.000000000000000000, 1.000000000000000000 ) ) ;
#5253 = CARTESIAN_POINT ( 'NONE',  ( 199.9999999999998863, 225.0000000000000284, 12.50000000000000000 ) ) ;
#5254 = CARTESIAN_POINT ( 'NONE',  ( 0.000000000000000000, 0.000000000000000000, 52.50000000000000000 ) ) ;
#5255 = EDGE_CURVE ( 'NONE', #7842, #5551, #7647, .T. ) ;
#5256 = DIRECTION ( 'NONE',  ( -0.000000000000000000, 0.000000000000000000, 1.000000000000000000 ) ) ;
#5257 =( REPRESENTATION_RELATIONSHIP ('NONE','NONE', #6292, #7467 ) REPRESENTATION_RELATIONSHIP_WITH_TRANSFORMATION ( #5748 )SHAPE_REPRESENTATION_RELATIONSHIP( ) );
#5258 = CARTESIAN_POINT ( 'NONE',  ( 387.1586741829164566, 19.78835583758980832, 2.930536303278098664 ) ) ;
#5259 = FACE_OUTER_BOUND ( 'NONE', #3702, .T. ) ;
#5260 = DIRECTION ( 'NONE',  ( -1.000000000000000000, -0.000000000000000000, -0.000000000000000000 ) ) ;
#5261 = ORIENTED_EDGE ( 'NONE', *, *, #5410, .T. ) ;
#5262 = ADVANCED_FACE ( 'NONE', ( #6680 ), #314, .F. ) ;
#5263 = CARTESIAN_POINT ( 'NONE',  ( -12.50000000000000000, 0.000000000000000000, -25.00000000000000000 ) ) ;
#5264 = DIRECTION ( 'NONE',  ( -0.000000000000000000, -0.000000000000000000, -1.000000000000000000 ) ) ;
#5265 = LINE ( 'NONE', #1179, #7230 ) ;
#5266 = SURFACE_STYLE_USAGE ( .BOTH. , #2750 ) ;
#5267 = VERTEX_POINT ( 'NONE', #3410 ) ;
#5268 = ADVANCED_FACE ( 'NONE', ( #4867 ), #5815, .T. ) ;
#5269 = PRODUCT_DEFINITION_SHAPE ( 'NONE', 'NONE',  #2123 ) ;
#5270 = AXIS2_PLACEMENT_3D ( 'NONE', #2663, #6312, #930 ) ;
#5271 = UNCERTAINTY_MEASURE_WITH_UNIT (LENGTH_MEASURE( 1.000000000000000082E-05 ), #94, 'distance_accuracy_value', 'NONE');
#5272 = ORIENTED_EDGE ( 'NONE', *, *, #946, .F. ) ;
#5273 = ADVANCED_FACE ( 'NONE', ( #592 ), #2854, .T. ) ;
#5274 = EDGE_LOOP ( 'NONE', ( #6043, #1596, #3433, #4391 ) ) ;
#5275 = VECTOR ( 'NONE', #6824, 1000.000000000000000 ) ;
#5276 = LINE ( 'NONE', #941, #6108 ) ;
#5277 = DIRECTION ( 'NONE',  ( -1.000000000000000000, 0.000000000000000000, 0.000000000000000000 ) ) ;
#5278 = ORIENTED_EDGE ( 'NONE', *, *, #4971, .F. ) ;
#5279 = FACE_OUTER_BOUND ( 'NONE', #3732, .T. ) ;
#5280 = DIRECTION ( 'NONE',  ( 1.000000000000000000, 0.000000000000000000, 0.000000000000000000 ) ) ;
#5281 = ORIENTED_EDGE ( 'NONE', *, *, #2085, .F. ) ;
#5282 = CARTESIAN_POINT ( 'NONE',  ( 46.25000000000002842, 79.24999999999990052, 130.0000000000000000 ) ) ;
#5283 = ORIENTED_EDGE ( 'NONE', *, *, #4634, .F. ) ;
#5284 = CARTESIAN_POINT ( 'NONE',  ( 0.000000000000000000, 0.000000000000000000, 0.000000000000000000 ) ) ;
#5285 = ORIENTED_EDGE ( 'NONE', *, *, #5391, .T. ) ;
#5286 = DIRECTION ( 'NONE',  ( -0.000000000000000000, 0.000000000000000000, 1.000000000000000000 ) ) ;
#5287 = ADVANCED_FACE ( 'NONE', ( #5480, #5898, #3000 ), #6810, .T. ) ;
#5288 = CARTESIAN_POINT ( 'NONE',  ( -27.49999999999989342, 177.4999999999999432, 12.50000000000000000 ) ) ;
#5289 = DIRECTION ( 'NONE',  ( 1.000000000000000000, 0.000000000000000000, 0.000000000000000000 ) ) ;
#5290 = CARTESIAN_POINT ( 'NONE',  ( 200.0000000000000000, -37.50000000000000711, 12.50000000000000000 ) ) ;
#5291 = ORIENTED_EDGE ( 'NONE', *, *, #6076, .T. ) ;
#5292 = EDGE_LOOP ( 'NONE', ( #6333, #257, #4992, #7057 ) ) ;
#5293 = EDGE_CURVE ( 'NONE', #1677, #2843, #5358, .T. ) ;
#5294 = DIRECTION ( 'NONE',  ( 1.000000000000000000, 0.000000000000000000, 0.000000000000000000 ) ) ;
#5295 = DIRECTION ( 'NONE',  ( 1.000000000000000000, 1.480297366166874072E-15, 0.000000000000000000 ) ) ;
#5296 = FACE_OUTER_BOUND ( 'NONE', #6024, .T. ) ;
#5297 = AXIS2_PLACEMENT_3D ( 'NONE', #6466, #5752, #256 ) ;
#5298 = CARTESIAN_POINT ( 'NONE',  ( 0.000000000000000000, 0.000000000000000000, 0.000000000000000000 ) ) ;
#5299 = CARTESIAN_POINT ( 'NONE',  ( 375.8471921630161887, 15.61249499599599844, 12.50000000000001066 ) ) ;
#5300 = CIRCLE ( 'NONE', #5702, 12.50000000000000355 ) ;
#5301 = AXIS2_PLACEMENT_3D ( 'NONE', #4104, #2384, #5916 ) ;
#5302 = DIRECTION ( 'NONE',  ( 1.000000000000000000, 0.000000000000000000, 0.000000000000000000 ) ) ;
#5303 = SHAPE_DEFINITION_REPRESENTATION ( #6423, #7467 ) ;
#5304 = ORIENTED_EDGE ( 'NONE', *, *, #3676, .F. ) ;
#5305 = DIRECTION ( 'NONE',  ( -0.000000000000000000, -0.000000000000000000, -1.000000000000000000 ) ) ;
#5306 = CARTESIAN_POINT ( 'NONE',  ( -31.24999999999997158, 47.50000000000009237, 130.0000000000000000 ) ) ;
#5307 = FACE_BOUND ( 'NONE', #3826, .T. ) ;
#5308 = ORIENTED_EDGE ( 'NONE', *, *, #2498, .F. ) ;
#5309 = VECTOR ( 'NONE', #6932, 1000.000000000000000 ) ;
#5310 = AXIS2_PLACEMENT_3D ( 'NONE', #6683, #1002, #3457 ) ;
#5311 = VECTOR ( 'NONE', #657, 1000.000000000000000 ) ;
#5312 = PRODUCT_RELATED_PRODUCT_CATEGORY ( 'part', '', ( #2127 ) ) ;
#5313 = ORIENTED_EDGE ( 'NONE', *, *, #3892, .F. ) ;
#5314 = AXIS2_PLACEMENT_3D ( 'NONE', #3503, #7755, #6467 ) ;
#5315 = EDGE_CURVE ( 'NONE', #3842, #2150, #5215, .T. ) ;
#5316 = EDGE_LOOP ( 'NONE', ( #2015, #63 ) ) ;
#5317 = SURFACE_STYLE_FILL_AREA ( #3482 ) ;
#5318 = LINE ( 'NONE', #7770, #7855 ) ;
#5319 = ORIENTED_EDGE ( 'NONE', *, *, #2213, .F. ) ;
#5320 = FILL_AREA_STYLE_COLOUR ( '', #4580 ) ;
#5321 = DIRECTION ( 'NONE',  ( 1.000000000000000000, 0.000000000000000000, 0.000000000000000000 ) ) ;
#5322 = CIRCLE ( 'NONE', #4928, 24.99999996734539920 ) ;
#5323 = ADVANCED_FACE ( 'NONE', ( #4640 ), #3597, .T. ) ;
#5324 = EDGE_CURVE ( 'NONE', #4430, #1115, #5869, .T. ) ;
#5325 = EDGE_LOOP ( 'NONE', ( #1869, #1988 ) ) ;
#5326 = EDGE_CURVE ( 'NONE', #342, #5607, #1764, .T. ) ;
#5327 = DIRECTION ( 'NONE',  ( -0.000000000000000000, -0.000000000000000000, 1.000000000000000000 ) ) ;
#5328 = ORIENTED_EDGE ( 'NONE', *, *, #7575, .F. ) ;
#5329 = DIRECTION ( 'NONE',  ( 0.000000000000000000, 0.000000000000000000, -1.000000000000000000 ) ) ;
#5330 = AXIS2_PLACEMENT_3D ( 'NONE', #712, #5687, #5611 ) ;
#5331 = EDGE_LOOP ( 'NONE', ( #1244, #4241, #2774, #7140 ) ) ;
#5332 = PLANE ( 'NONE',  #1001 ) ;
#5333 = DIRECTION ( 'NONE',  ( -0.000000000000000000, -0.000000000000000000, -1.000000000000000000 ) ) ;
#5334 = EDGE_CURVE ( 'NONE', #6102, #2325, #99, .T. ) ;
#5335 = PRESENTATION_LAYER_ASSIGNMENT (  '', '', ( #1358 ) ) ;
#5336 = ORIENTED_EDGE ( 'NONE', *, *, #4730, .T. ) ;
#5337 = ORIENTED_EDGE ( 'NONE', *, *, #127, .F. ) ;
#5338 = PRODUCT_DEFINITION_SHAPE ( 'NONE', 'NONE',  #7934 ) ;
#5339 = DIRECTION ( 'NONE',  ( -0.000000000000000000, -0.000000000000000000, 1.000000000000000000 ) ) ;
#5340 = CARTESIAN_POINT ( 'NONE',  ( -12.50000000000000000, 0.000000000000000000, 25.00000000000000000 ) ) ;
#5342 = CARTESIAN_POINT ( 'NONE',  ( -6.495190528383282036, -11.24999999999999645, 0.000000000000000000 ) ) ;
#5341 = CIRCLE ( 'NONE', #1752, 12.50000000000001066 ) ;
#5343 = FACE_OUTER_BOUND ( 'NONE', #3916, .T. ) ;
#5344 = CARTESIAN_POINT ( 'NONE',  ( 381.3043660624298923, 16.83403191367835561, 10.80131548116625417 ) ) ;
#5345 = ADVANCED_FACE ( 'NONE', ( #7253 ), #7326, .T. ) ;
#5346 = AXIS2_PLACEMENT_3D ( 'NONE', #4984, #6229, #4938 ) ;
#5347 = CARTESIAN_POINT ( 'NONE',  ( -37.49999999999997158, 1.601283208593976678E-14, 12.50000000000000000 ) ) ;
#5348 = APPLICATION_PROTOCOL_DEFINITION ( 'draft international standard', 'automotive_design', 1998, #1516 ) ;
#5349 = VERTEX_POINT ( 'NONE', #175 ) ;
#5350 = CYLINDRICAL_SURFACE ( 'NONE', #2546, 5.000000000000000000 ) ;
#5351 = CARTESIAN_POINT ( 'NONE',  ( 17.32050807568877104, 2.500000000000000888, 7.500000000000000000 ) ) ;
#5352 = DIRECTION ( 'NONE',  ( -1.000000000000000000, -0.000000000000000000, -0.000000000000000000 ) ) ;
#5353 = ORIENTED_EDGE ( 'NONE', *, *, #1165, .F. ) ;
#5354 = AXIS2_PLACEMENT_3D ( 'NONE', #4250, #1922, #532 ) ;
#5355 = EDGE_LOOP ( 'NONE', ( #250, #2917, #2652, #5328 ) ) ;
#5356 = ORIENTED_EDGE ( 'NONE', *, *, #1612, .F. ) ;
#5357 = VECTOR ( 'NONE', #1376, 1000.000000000000114 ) ;
#5358 = CIRCLE ( 'NONE', #1004, 17.50000000000000355 ) ;
#5359 = APPLICATION_CONTEXT ( 'automotive_design' ) ;
#5360 = VERTEX_POINT ( 'NONE', #7365 ) ;
#5361 = DIRECTION ( 'NONE',  ( 0.000000000000000000, 0.000000000000000000, 1.000000000000000000 ) ) ;
#5362 = CYLINDRICAL_SURFACE ( 'NONE', #4521, 5.000000000000000000 ) ;
#5363 = ORIENTED_EDGE ( 'NONE', *, *, #5334, .T. ) ;
#5364 = LINE ( 'NONE', #2967, #3908 ) ;
#5365 = AXIS2_PLACEMENT_3D ( 'NONE', #3504, #4654, #376 ) ;
#5366 = VECTOR ( 'NONE', #6521, 1000.000000000000000 ) ;
#5367 = ORIENTED_EDGE ( 'NONE', *, *, #6747, .F. ) ;
#5368 = CARTESIAN_POINT ( 'NONE',  ( 326.6025403784437913, 75.00000000000005684, 125.0000000000000000 ) ) ;
#5369 = ORIENTED_EDGE ( 'NONE', *, *, #346, .T. ) ;
#5370 = VECTOR ( 'NONE', #1814, 1000.000000000000114 ) ;
#5371 = CARTESIAN_POINT ( 'NONE',  ( -25.00000000000000000, 0.000000000000000000, 0.000000000000000000 ) ) ;
#5372 = CONICAL_SURFACE ( 'NONE', #7037, 15.00000000000000000, 0.7853981633974479459 ) ;
#5373 = ORIENTED_EDGE ( 'NONE', *, *, #4050, .T. ) ;
#5374 = ADVANCED_FACE ( 'NONE', ( #5678 ), #5024, .F. ) ;
#5375 = DIRECTION ( 'NONE',  ( 0.000000000000000000, 0.000000000000000000, -1.000000000000000000 ) ) ;
#5376 = CARTESIAN_POINT ( 'NONE',  ( 0.000000000000000000, 262.5000000000000568, 12.50000000000000000 ) ) ;
#5377 = ADVANCED_FACE ( 'NONE', ( #1938 ), #7479, .F. ) ;
#5378 = ORIENTED_EDGE ( 'NONE', *, *, #3608, .T. ) ;
#5379 = ORIENTED_EDGE ( 'NONE', *, *, #1802, .F. ) ;
#5380 = EDGE_CURVE ( 'NONE', #4458, #3990, #7445, .T. ) ;
#5381 = DIRECTION ( 'NONE',  ( 1.000000000000000000, 1.040834085586084257E-15, 0.000000000000000000 ) ) ;
#5382 = CARTESIAN_POINT ( 'NONE',  ( 175.0000000000000000, 0.000000000000000000, 15.00000000000000000 ) ) ;
#5383 = CARTESIAN_POINT ( 'NONE',  ( 296.6025403784437913, 137.4999999999999716, 17.49999999999998934 ) ) ;
#5384 = CARTESIAN_POINT ( 'NONE',  ( 5.204170427930428856E-14, 37.50000000000005684, 0.000000000000000000 ) ) ;
#5385 = CARTESIAN_POINT ( 'NONE',  ( -17.32050807568877104, -2.499999999999999112, 0.000000000000000000 ) ) ;
#5386 = DIRECTION ( 'NONE',  ( 1.000000000000000000, 0.000000000000000000, 0.000000000000000000 ) ) ;
#5387 = PRODUCT_CONTEXT ( 'NONE', #5359, 'mechanical' ) ;
#5388 = B_SPLINE_CURVE_WITH_KNOTS ( 'NONE', 3,
 ( #3865, #5176, #774, #3827 ),
 .UNSPECIFIED., .F., .F.,
 ( 4, 4 ),
 ( 1.734723475976807094E-18, 0.003328530869593415188 ),
 .UNSPECIFIED. ) ;
#5389 = DIRECTION ( 'NONE',  ( -1.000000000000000000, 0.000000000000000000, 0.000000000000000000 ) ) ;
#5390 = DIRECTION ( 'NONE',  ( -0.000000000000000000, 0.000000000000000000, 1.000000000000000000 ) ) ;
#5391 = EDGE_CURVE ( 'NONE', #1141, #6641, #1228, .T. ) ;
#5392 = LINE ( 'NONE', #7838, #564 ) ;
#5393 = ORIENTED_EDGE ( 'NONE', *, *, #7487, .F. ) ;
#5394 = VECTOR ( 'NONE', #2190, 1000.000000000000000 ) ;
#5395 = ORIENTED_EDGE ( 'NONE', *, *, #2242, .T. ) ;
#5396 = ORIENTED_EDGE ( 'NONE', *, *, #5910, .T. ) ;
#5397 = PRESENTATION_STYLE_ASSIGNMENT (( #2964 ) ) ;
#5398 = DIRECTION ( 'NONE',  ( -4.789677997474686366E-16, -1.000000000000000000, -0.000000000000000000 ) ) ;
#5399 = AXIS2_PLACEMENT_3D ( 'NONE', #2017, #7674, #2178 ) ;
#5400 = ORIENTED_EDGE ( 'NONE', *, *, #2775, .F. ) ;
#5401 = DIRECTION ( 'NONE',  ( -0.000000000000000000, -0.000000000000000000, -1.000000000000000000 ) ) ;
#5402 = VERTEX_POINT ( 'NONE', #6880 ) ;
#5403 = LINE ( 'NONE', #2930, #117 ) ;
#5404 = ORIENTED_EDGE ( 'NONE', *, *, #2548, .T. ) ;
#5405 = CARTESIAN_POINT ( 'NONE',  ( 362.4984763656763107, -20.00095227047670576, -0.8223324121160918709 ) ) ;
#5406 = EDGE_LOOP ( 'NONE', ( #2664, #7768, #5400, #2399, #6435, #6530, #6907 ) ) ;
#5407 = CARTESIAN_POINT ( 'NONE',  ( 190.0000000000000000, 0.000000000000000000, 0.000000000000000000 ) ) ;
#5408 = CARTESIAN_POINT ( 'NONE',  ( -25.00000000000000000, 0.000000000000000000, 0.000000000000000000 ) ) ;
#5409 = VERTEX_POINT ( 'NONE', #6717 ) ;
#5410 = EDGE_CURVE ( 'NONE', #5409, #4474, #3758, .T. ) ;
#5411 = ORIENTED_EDGE ( 'NONE', *, *, #6750, .F. ) ;
#5412 = EDGE_CURVE ( 'NONE', #6817, #3835, #3818, .T. ) ;
#5413 = FACE_OUTER_BOUND ( 'NONE', #3229, .T. ) ;
#5414 = FACE_OUTER_BOUND ( 'NONE', #999, .T. ) ;
#5415 = CARTESIAN_POINT ( 'NONE',  ( -12.50000000000000000, 0.000000000000000000, 2.500000000000085265 ) ) ;
#5416 = CARTESIAN_POINT ( 'NONE',  ( 13.21904415029483459, 19.40417101989674009, 12.50000000000000000 ) ) ;
#5417 = CARTESIAN_POINT ( 'NONE',  ( 412.4999999999998295, 145.0000000000000284, 5.000000000000000000 ) ) ;
#5418 = CARTESIAN_POINT ( 'NONE',  ( 291.6025403784437913, 135.0000000000000000, 12.50000000000000000 ) ) ;
#5419 = EDGE_CURVE ( 'NONE', #7620, #3810, #2412, .T. ) ;
#5420 = EDGE_CURVE ( 'NONE', #4679, #2146, #6237, .T. ) ;
#5421 = CYLINDRICAL_SURFACE ( 'NONE', #1777, 12.50000000000001066 ) ;
#5422 = AXIS2_PLACEMENT_3D ( 'NONE', #6039, #3549, #1219 ) ;
#5423 =( NAMED_UNIT ( * ) SI_UNIT ( $, .STERADIAN. ) SOLID_ANGLE_UNIT ( ) );
#5424 = CIRCLE ( 'NONE', #1962, 12.50000000000001776 ) ;
#5425 = CARTESIAN_POINT ( 'NONE',  ( 12.50000000000000000, 1.530808498934191127E-15, 90.00000000000000000 ) ) ;
#5426 = CYLINDRICAL_SURFACE ( 'NONE', #5820, 12.50000000000000355 ) ;
#5427 = CARTESIAN_POINT ( 'NONE',  ( 150.0000000000000000, 1.836970198721029747E-14, 25.00000000000000000 ) ) ;
#5428 = ORIENTED_EDGE ( 'NONE', *, *, #5807, .T. ) ;
#5429 = ADVANCED_FACE ( 'NONE', ( #4346 ), #4308, .F. ) ;
#5430 = AXIS2_PLACEMENT_3D ( 'NONE', #4693, #5170, #7625 ) ;
#5431 = PRODUCT_DEFINITION_CONTEXT ( 'detailed design', #6650, 'design' ) ;
#5432 = AXIS2_PLACEMENT_3D ( 'NONE', #3590, #5878, #382 ) ;
#5433 = ORIENTED_EDGE ( 'NONE', *, *, #7784, .T. ) ;
#5434 =( LENGTH_UNIT ( ) NAMED_UNIT ( * ) SI_UNIT ( .MILLI., .METRE. ) );
#5435 = ORIENTED_EDGE ( 'NONE', *, *, #3081, .T. ) ;
#5436 = DIRECTION ( 'NONE',  ( -0.000000000000000000, -0.000000000000000000, -1.000000000000000000 ) ) ;
#5437 = DIRECTION ( 'NONE',  ( 0.000000000000000000, 0.000000000000000000, 1.000000000000000000 ) ) ;
#5439 = FACE_OUTER_BOUND ( 'NONE', #2996, .T. ) ;
#5438 = CIRCLE ( 'NONE', #1970, 9.999999999999896971 ) ;
#5440 = AXIS2_PLACEMENT_3D ( 'NONE', #3950, #981, #7167 ) ;
#5441 = AXIS2_PLACEMENT_3D ( 'NONE', #1445, #255, #807 ) ;
#5442 = EDGE_LOOP ( 'NONE', ( #2067, #5842, #4488, #6527 ) ) ;
#5443 = CARTESIAN_POINT ( 'NONE',  ( 0.000000000000000000, 0.000000000000000000, 0.000000000000000000 ) ) ;
#5444 = VECTOR ( 'NONE', #7853, 1000.000000000000000 ) ;
#5445 = CIRCLE ( 'NONE', #1981, 5.000000000000000000 ) ;
#5446 = ORIENTED_EDGE ( 'NONE', *, *, #7726, .F. ) ;
#5447 = CIRCLE ( 'NONE', #7496, 5.000000000000000000 ) ;
#5448 = ADVANCED_FACE ( 'NONE', ( #3195 ), #6199, .T. ) ;
#5449 = CARTESIAN_POINT ( 'NONE',  ( 412.4999999999998863, 142.5000000000000000, 155.0000000000000000 ) ) ;
#5450 = VERTEX_POINT ( 'NONE', #2586 ) ;
#5451 = CARTESIAN_POINT ( 'NONE',  ( 362.6101369827622420, -19.93132096080314497, 1.708129828930195826 ) ) ;
#5452 = ORIENTED_EDGE ( 'NONE', *, *, #7285, .F. ) ;
#5453 = DIRECTION ( 'NONE',  ( -0.000000000000000000, -0.000000000000000000, -1.000000000000000000 ) ) ;
#5454 = CIRCLE ( 'NONE', #2378, 5.000000000000000000 ) ;
#5455 = CARTESIAN_POINT ( 'NONE',  ( 6.495190528383288253, -16.24999999999999645, 0.000000000000000000 ) ) ;
#5456 = ORIENTED_EDGE ( 'NONE', *, *, #2036, .T. ) ;
#5457 = AXIS2_PLACEMENT_3D ( 'NONE', #7604, #7769, #4553 ) ;
#5458 = ORIENTED_EDGE ( 'NONE', *, *, #33, .T. ) ;
#5459 = CARTESIAN_POINT ( 'NONE',  ( -17.32050807568877104, 2.500000000000002220, 0.000000000000000000 ) ) ;
#5460 = FACE_OUTER_BOUND ( 'NONE', #5186, .T. ) ;
#5461 = DIRECTION ( 'NONE',  ( 1.000000000000000000, 0.000000000000000000, -0.000000000000000000 ) ) ;
#5462 = CARTESIAN_POINT ( 'NONE',  ( -66.45428044951677293, 30.87346046883880035, 12.50000000000000000 ) ) ;
#5463 = DIRECTION ( 'NONE',  ( 0.000000000000000000, 0.000000000000000000, -1.000000000000000000 ) ) ;
#5464 = CIRCLE ( 'NONE', #3677, 12.50000000000001066 ) ;
#5465 = DIRECTION ( 'NONE',  ( -0.000000000000000000, -0.000000000000000000, -1.000000000000000000 ) ) ;
#5466 = DIRECTION ( 'NONE',  ( 1.000000000000000000, 0.000000000000000000, 0.000000000000000000 ) ) ;
#5467 = CIRCLE ( 'NONE', #7004, 12.50000000000000000 ) ;
#5468 = CONTEXT_DEPENDENT_SHAPE_REPRESENTATION ( #2699, #7637 ) ;
#5469 = DIRECTION ( 'NONE',  ( -0.000000000000000000, -0.000000000000000000, -1.000000000000000000 ) ) ;
#5470 = DIRECTION ( 'NONE',  ( -0.000000000000000000, -0.000000000000000000, 1.000000000000000000 ) ) ;
#5471 = CARTESIAN_POINT ( 'NONE',  ( 6.495190528383289141, -11.24999999999999645, 0.000000000000000000 ) ) ;
#5472 = DIRECTION ( 'NONE',  ( 0.000000000000000000, 1.000000000000000000, 0.000000000000000000 ) ) ;
#5473 = EDGE_CURVE ( 'NONE', #994, #4917, #362, .T. ) ;
#5474 = AXIS2_PLACEMENT_3D ( 'NONE', #2944, #6624, #5381 ) ;
#5475 = EDGE_CURVE ( 'NONE', #5267, #5496, #7406, .T. ) ;
#5476 = ORIENTED_EDGE ( 'NONE', *, *, #2823, .F. ) ;
#5477 =( NAMED_UNIT ( * ) SI_UNIT ( $, .STERADIAN. ) SOLID_ANGLE_UNIT ( ) );
#5478 = VERTEX_POINT ( 'NONE', #6162 ) ;
#5479 = CARTESIAN_POINT ( 'NONE',  ( 25.71904415029483459, -5.595828947448873159, 12.50000000000000000 ) ) ;
#5480 = FACE_BOUND ( 'NONE', #5814, .T. ) ;
#5481 = CIRCLE ( 'NONE', #993, 25.00000000000000000 ) ;
#5482 = DIRECTION ( 'NONE',  ( -4.789677997474686366E-16, -1.000000000000000000, -0.000000000000000000 ) ) ;
#5483 = CYLINDRICAL_SURFACE ( 'NONE', #50, 25.00000000000000000 ) ;
#5484 = ORIENTED_EDGE ( 'NONE', *, *, #2187, .T. ) ;
#5485 = DIRECTION ( 'NONE',  ( 4.237492460401360996E-16, 1.000000000000000000, -8.474984920802721991E-16 ) ) ;
#5486 = AXIS2_PLACEMENT_3D ( 'NONE', #3291, #5782, #5375 ) ;
#5487 = VECTOR ( 'NONE', #140, 1000.000000000000000 ) ;
#5488 = ORIENTED_EDGE ( 'NONE', *, *, #3102, .F. ) ;
#5489 = LINE ( 'NONE', #6052, #6016 ) ;
#5490 = ORIENTED_EDGE ( 'NONE', *, *, #1163, .F. ) ;
#5491 = CARTESIAN_POINT ( 'NONE',  ( 374.1492488978694837, -15.62998136526340076, -12.47825053757332370 ) ) ;
#5492 = ORIENTED_EDGE ( 'NONE', *, *, #2293, .F. ) ;
#5493 = CARTESIAN_POINT ( 'NONE',  ( 12.50000000000000355, 0.000000000000000000, 97.50000000000000000 ) ) ;
#5494 = DIRECTION ( 'NONE',  ( -1.000000000000000000, 4.270088556250607616E-16, -0.000000000000000000 ) ) ;
#5495 = EDGE_CURVE ( 'NONE', #2143, #5042, #54, .T. ) ;
#5496 = VERTEX_POINT ( 'NONE', #1305 ) ;
#5497 = AXIS2_PLACEMENT_3D ( 'NONE', #6705, #3668, #3108 ) ;
#5498 = VECTOR ( 'NONE', #2215, 1000.000000000000000 ) ;
#5499 = ORIENTED_EDGE ( 'NONE', *, *, #5766, .F. ) ;
#5500 = ORIENTED_EDGE ( 'NONE', *, *, #4771, .T. ) ;
#5501 = CARTESIAN_POINT ( 'NONE',  ( 0.000000000000000000, 0.000000000000000000, 52.50000000000000000 ) ) ;
#5502 = DIRECTION ( 'NONE',  ( 1.000000000000000000, 0.000000000000000000, 0.000000000000000000 ) ) ;
#5503 = DIRECTION ( 'NONE',  ( 0.5000000000000001110, -0.8660254037844385966, 0.000000000000000000 ) ) ;
#5504 = CARTESIAN_POINT ( 'NONE',  ( 0.000000000000000000, 0.000000000000000000, 25.00000000000000000 ) ) ;
#5505 = DIRECTION ( 'NONE',  ( 1.224646799147353207E-16, 1.000000000000000000, 0.000000000000000000 ) ) ;
#5506 = VECTOR ( 'NONE', #5327, 1000.000000000000000 ) ;
#5507 = CARTESIAN_POINT ( 'NONE',  ( 382.6349272670254322, 17.37719324208310923, -9.905392396107414399 ) ) ;
#5508 = DIRECTION ( 'NONE',  ( -0.000000000000000000, -0.000000000000000000, 1.000000000000000000 ) ) ;
#5509 = ADVANCED_FACE ( 'NONE', ( #3156 ), #98, .F. ) ;
#5510 = LINE ( 'NONE', #6753, #5099 ) ;
#5511 = DIRECTION ( 'NONE',  ( 0.000000000000000000, -0.000000000000000000, 1.000000000000000000 ) ) ;
#5512 = CARTESIAN_POINT ( 'NONE',  ( -12.50000000000000000, -24.99999999999999645, 3.851859888774471706E-31 ) ) ;
#5513 = ORIENTED_EDGE ( 'NONE', *, *, #3406, .F. ) ;
#5514 = EDGE_CURVE ( 'NONE', #7523, #393, #5643, .T. ) ;
#5515 =( NAMED_UNIT ( * ) SI_UNIT ( $, .STERADIAN. ) SOLID_ANGLE_UNIT ( ) );
#5516 = VERTEX_POINT ( 'NONE', #1499 ) ;
#5517 = DIRECTION ( 'NONE',  ( 0.000000000000000000, 0.000000000000000000, 1.000000000000000000 ) ) ;
#5518 = DIRECTION ( 'NONE',  ( -1.000000000000000000, 0.000000000000000000, 0.000000000000000000 ) ) ;
#5519 = DIRECTION ( 'NONE',  ( -0.000000000000000000, 0.000000000000000000, 1.000000000000000000 ) ) ;
#5520 = EDGE_CURVE ( 'NONE', #3451, #5068, #3907, .T. ) ;
#5521 = CARTESIAN_POINT ( 'NONE',  ( -31.24999999999997158, 111.9999999999999289, 130.0000000000000000 ) ) ;
#5522 = ORIENTED_EDGE ( 'NONE', *, *, #5962, .T. ) ;
#5523 = AXIS2_PLACEMENT_3D ( 'NONE', #3396, #3989, #904 ) ;
#5524 = FACE_OUTER_BOUND ( 'NONE', #7448, .T. ) ;
#5525 = UNCERTAINTY_MEASURE_WITH_UNIT (LENGTH_MEASURE( 1.000000000000000082E-05 ), #5434, 'distance_accuracy_value', 'NONE');
#5526 = EDGE_CURVE ( 'NONE', #3736, #781, #7412, .T. ) ;
#5527 = VERTEX_POINT ( 'NONE', #217 ) ;
#5528 = CARTESIAN_POINT ( 'NONE',  ( 372.9002586711609410, 15.74791738283697740, 12.32940567573685087 ) ) ;
#5529 = EDGE_LOOP ( 'NONE', ( #5404, #4385 ) ) ;
#5530 = CARTESIAN_POINT ( 'NONE',  ( 368.3509586464906533, -16.96668907523693548, 10.59241602951089867 ) ) ;
#5531 = ORIENTED_EDGE ( 'NONE', *, *, #2078, .T. ) ;
#5532 = CARTESIAN_POINT ( 'NONE',  ( 0.000000000000000000, 0.000000000000000000, 0.5000000000000004441 ) ) ;
#5533 = EDGE_LOOP ( 'NONE', ( #2592, #6421 ) ) ;
#5534 = EDGE_LOOP ( 'NONE', ( #1308, #6408, #6976, #1425 ) ) ;
#5535 = ORIENTED_EDGE ( 'NONE', *, *, #5118, .T. ) ;
#5536 = CARTESIAN_POINT ( 'NONE',  ( 384.3872655588493785, -18.21073727249144625, 8.292169370763099678 ) ) ;
#5537 = AXIS2_PLACEMENT_3D ( 'NONE', #5504, #1843, #4934 ) ;
#5538 = CARTESIAN_POINT ( 'NONE',  ( 387.4799551155421682, -19.98745133777255134, 0.8232361438305751955 ) ) ;
#5539 = CARTESIAN_POINT ( 'NONE',  ( -6.495190528383282036, -16.24999999999999645, 7.500000000000000000 ) ) ;
#5540 = DIRECTION ( 'NONE',  ( 0.000000000000000000, 0.000000000000000000, -1.000000000000000000 ) ) ;
#5541 = DIRECTION ( 'NONE',  ( 1.000000000000000000, 0.000000000000000000, 0.000000000000000000 ) ) ;
#5542 = EDGE_CURVE ( 'NONE', #1637, #3100, #293, .T. ) ;
#5543 = CARTESIAN_POINT ( 'NONE',  ( 15.00000000000000000, 0.000000000000000000, 52.50000000000000000 ) ) ;
#5544 = ITEM_DEFINED_TRANSFORMATION ( 'NONE', 'NONE', #149,  #5785 ) ;
#5545 = CARTESIAN_POINT ( 'NONE',  ( 286.6025403784439050, 90.00000000000001421, 12.50000000000000000 ) ) ;
#5546 = LINE ( 'NONE', #4861, #3709 ) ;
#5547 = DIRECTION ( 'NONE',  ( -0.000000000000000000, 0.000000000000000000, -1.000000000000000000 ) ) ;
#5548 = DIRECTION ( 'NONE',  ( -0.000000000000000000, -0.000000000000000000, -1.000000000000000000 ) ) ;
#5549 = ORIENTED_EDGE ( 'NONE', *, *, #2109, .T. ) ;
#5550 =( NAMED_UNIT ( * ) SI_UNIT ( $, .STERADIAN. ) SOLID_ANGLE_UNIT ( ) );
#5551 = VERTEX_POINT ( 'NONE', #978 ) ;
#5552 =( NAMED_UNIT ( * ) PLANE_ANGLE_UNIT ( ) SI_UNIT ( $, .RADIAN. ) );
#5553 = DIRECTION ( 'NONE',  ( 1.000000000000000000, 0.000000000000000000, 0.000000000000000000 ) ) ;
#5554 = DIRECTION ( 'NONE',  ( 0.000000000000000000, -0.000000000000000000, 1.000000000000000000 ) ) ;
#5555 = CARTESIAN_POINT ( 'NONE',  ( 200.0000000000000000, 0.000000000000000000, 0.000000000000000000 ) ) ;
#5556 = ORIENTED_EDGE ( 'NONE', *, *, #6651, .F. ) ;
#5557 = AXIS2_PLACEMENT_3D ( 'NONE', #2948, #2375, #4812 ) ;
#5558 =( GEOMETRIC_REPRESENTATION_CONTEXT ( 3 ) GLOBAL_UNCERTAINTY_ASSIGNED_CONTEXT ( ( #6807 ) ) GLOBAL_UNIT_ASSIGNED_CONTEXT ( ( #4486, #7699, #4641 ) ) REPRESENTATION_CONTEXT ( 'NONE', 'WORKASPACE' ) );
#5559 = CARTESIAN_POINT ( 'NONE',  ( 0.000000000000000000, 0.000000000000000000, 200.0000000000000000 ) ) ;
#5560 = AXIS2_PLACEMENT_3D ( 'NONE', #1862, #3833, #21 ) ;
#5561 = EDGE_CURVE ( 'NONE', #3167, #3644, #5761, .T. ) ;
#5562 = EDGE_CURVE ( 'NONE', #5860, #6805, #5876, .T. ) ;
#5563 = VERTEX_POINT ( 'NONE', #6396 ) ;
#5564 = AXIS2_PLACEMENT_3D ( 'NONE', #1683, #7785, #3649 ) ;
#5565 = CARTESIAN_POINT ( 'NONE',  ( 364.2021130961084623, 18.97902931052027142, -6.348195341973490891 ) ) ;
#5566 = VECTOR ( 'NONE', #5140, 1000.000000000000000 ) ;
#5567 = ORIENTED_EDGE ( 'NONE', *, *, #4875, .T. ) ;
#5568 = DIRECTION ( 'NONE',  ( 0.000000000000000000, 0.000000000000000000, 1.000000000000000000 ) ) ;
#5569 = VERTEX_POINT ( 'NONE', #5835 ) ;
#5570 = DIRECTION ( 'NONE',  ( 1.000000000000000000, 0.000000000000000000, 0.000000000000000000 ) ) ;
#5571 =( REPRESENTATION_RELATIONSHIP ('NONE','NONE', #6292, #7467 ) REPRESENTATION_RELATIONSHIP_WITH_TRANSFORMATION ( #1964 )SHAPE_REPRESENTATION_RELATIONSHIP( ) );
#5572 = EDGE_CURVE ( 'NONE', #2323, #3115, #6353, .T. ) ;
#5573 = VECTOR ( 'NONE', #1429, 1000.000000000000000 ) ;
#5574 = AXIS2_PLACEMENT_3D ( 'NONE', #1180, #3078, #2315 ) ;
#5575 = AXIS2_PLACEMENT_3D ( 'NONE', #5383, #1567, #4010 ) ;
#5576 = EDGE_CURVE ( 'NONE', #1704, #2, #7911, .T. ) ;
#5577 = EDGE_LOOP ( 'NONE', ( #5500, #5778, #464, #4438 ) ) ;
#5578 = VERTEX_POINT ( 'NONE', #3386 ) ;
#5579 = AXIS2_PLACEMENT_3D ( 'NONE', #6843, #3121, #4384 ) ;
#5580 = ORIENTED_EDGE ( 'NONE', *, *, #480, .F. ) ;
#5581 = CARTESIAN_POINT ( 'NONE',  ( -27.49999999999989342, 182.4999999999999432, 12.50000000000000000 ) ) ;
#5582 = EDGE_CURVE ( 'NONE', #221, #4039, #4450, .T. ) ;
#5583 = LINE ( 'NONE', #4888, #613 ) ;
#5584 = EDGE_CURVE ( 'NONE', #5686, #6926, #5222, .T. ) ;
#5585 = DIRECTION ( 'NONE',  ( 0.000000000000000000, 0.000000000000000000, -1.000000000000000000 ) ) ;
#5586 = FACE_OUTER_BOUND ( 'NONE', #4239, .T. ) ;
#5587 = CARTESIAN_POINT ( 'NONE',  ( -31.24999999999997158, 177.4999999999999432, 17.50000000000001421 ) ) ;
#5588 = CIRCLE ( 'NONE', #7883, 12.50000000000001066 ) ;
#5589 = APPLICATION_PROTOCOL_DEFINITION ( 'draft international standard', 'automotive_design', 1998, #1921 ) ;
#5590 = PLANE ( 'NONE',  #7401 ) ;
#5591 = CARTESIAN_POINT ( 'NONE',  ( -11.78095584970496290, 62.70544120911855401, 0.000000000000000000 ) ) ;
#5593 = CARTESIAN_POINT ( 'NONE',  ( 190.0000000000000000, 12.50000000000000000, 15.61249499599599488 ) ) ;
#5592 =( GEOMETRIC_REPRESENTATION_CONTEXT ( 3 ) GLOBAL_UNCERTAINTY_ASSIGNED_CONTEXT ( ( #638 ) ) GLOBAL_UNIT_ASSIGNED_CONTEXT ( ( #3084, #475, #3723 ) ) REPRESENTATION_CONTEXT ( 'NONE', 'WORKASPACE' ) );
#5594 = CYLINDRICAL_SURFACE ( 'NONE', #704, 20.00000000000000000 ) ;
#5595 = EDGE_CURVE ( 'NONE', #2226, #1787, #7677, .T. ) ;
#5596 = ORIENTED_EDGE ( 'NONE', *, *, #5816, .T. ) ;
#5597 = AXIS2_PLACEMENT_3D ( 'NONE', #1892, #6827, #1295 ) ;
#5598 = ORIENTED_EDGE ( 'NONE', *, *, #7439, .F. ) ;
#5599 = DIRECTION ( 'NONE',  ( 0.000000000000000000, 0.000000000000000000, -1.000000000000000000 ) ) ;
#5600 = CARTESIAN_POINT ( 'NONE',  ( -48.67326389759909944, 48.65950482248330644, 12.50000000000000000 ) ) ;
#5601 = LINE ( 'NONE', #4995, #1075 ) ;
#5602 = CARTESIAN_POINT ( 'NONE',  ( -25.00000000000000000, 0.000000000000000000, 25.00000000000000000 ) ) ;
#5603 = ORIENTED_EDGE ( 'NONE', *, *, #5154, .T. ) ;
#5604 = CONICAL_SURFACE ( 'NONE', #5990, 18.75000000000009948, 0.7853981633974421728 ) ;
#5605 = PLANE ( 'NONE',  #6732 ) ;
#5606 = UNCERTAINTY_MEASURE_WITH_UNIT (LENGTH_MEASURE( 1.000000000000000082E-05 ), #4459, 'distance_accuracy_value', 'NONE');
#5607 = VERTEX_POINT ( 'NONE', #3981 ) ;
#5608 = CIRCLE ( 'NONE', #7014, 5.000000000000000888 ) ;
#5609 = CARTESIAN_POINT ( 'NONE',  ( 296.6025403784439050, 82.50000000000004263, 125.0000000000000000 ) ) ;
#5610 = ORIENTED_EDGE ( 'NONE', *, *, #1254, .T. ) ;
#5611 = DIRECTION ( 'NONE',  ( 1.000000000000000000, 0.000000000000000000, 0.000000000000000000 ) ) ;
#5612 = EDGE_LOOP ( 'NONE', ( #3210, #1558, #1438, #4991 ) ) ;
#5613 = DIRECTION ( 'NONE',  ( -1.000000000000000000, 0.000000000000000000, 0.000000000000000000 ) ) ;
#5614 = LINE ( 'NONE', #791, #2625 ) ;
#5615 = CONICAL_SURFACE ( 'NONE', #739, 20.00000000000000000, 0.7853981633974578269 ) ;
#5616 = VECTOR ( 'NONE', #3348, 1000.000000000000000 ) ;
#5617 = ORIENTED_EDGE ( 'NONE', *, *, #5315, .F. ) ;
#5618 = ORIENTED_EDGE ( 'NONE', *, *, #3083, .T. ) ;
#5619 = VECTOR ( 'NONE', #6631, 1000.000000000000000 ) ;
#5620 = EDGE_CURVE ( 'NONE', #5607, #7342, #4618, .T. ) ;
#5621 = VECTOR ( 'NONE', #1852, 1000.000000000000000 ) ;
#5622 = ORIENTED_EDGE ( 'NONE', *, *, #5572, .T. ) ;
#5623 = DIRECTION ( 'NONE',  ( 0.000000000000000000, 0.000000000000000000, -1.000000000000000000 ) ) ;
#5624 = DIRECTION ( 'NONE',  ( -0.000000000000000000, -0.000000000000000000, -1.000000000000000000 ) ) ;
#5625 = CARTESIAN_POINT ( 'NONE',  ( 0.000000000000000000, 0.000000000000000000, 90.00000000000000000 ) ) ;
#5626 = DIRECTION ( 'NONE',  ( -4.789677997474686366E-16, -1.000000000000000000, -0.000000000000000000 ) ) ;
#5627 = EDGE_CURVE ( 'NONE', #161, #1161, #7517, .T. ) ;
#5628 = DIRECTION ( 'NONE',  ( 0.000000000000000000, 0.000000000000000000, 1.000000000000000000 ) ) ;
#5629 = AXIS2_PLACEMENT_3D ( 'NONE', #6332, #397, #2687 ) ;
#5630 = AXIS2_PLACEMENT_3D ( 'NONE', #457, #1048, #3500 ) ;
#5631 = CONTEXT_DEPENDENT_SHAPE_REPRESENTATION ( #901, #7003 ) ;
#5632 = CIRCLE ( 'NONE', #5889, 12.50000000000000000 ) ;
#5633 = DIRECTION ( 'NONE',  ( -0.000000000000000000, 0.000000000000000000, 1.000000000000000000 ) ) ;
#5634 = DIRECTION ( 'NONE',  ( 1.000000000000000000, 0.000000000000000000, 0.000000000000000000 ) ) ;
#5635 = CIRCLE ( 'NONE', #1779, 25.00000000000000000 ) ;
#5636 = CARTESIAN_POINT ( 'NONE',  ( 10.82531754730547213, 13.75000000000000178, 7.500000000000000000 ) ) ;
#5637 = LINE ( 'NONE', #3258, #1197 ) ;
#5638 = VERTEX_POINT ( 'NONE', #2098 ) ;
#5639 = LINE ( 'NONE', #5135, #365 ) ;
#5640 = ORIENTED_EDGE ( 'NONE', *, *, #7251, .T. ) ;
#5641 = ADVANCED_FACE ( 'NONE', ( #7041 ), #7534, .T. ) ;
#5642 = LINE ( 'NONE', #5063, #3545 ) ;
#5643 = LINE ( 'NONE', #857, #5746 ) ;
#5644 = DIRECTION ( 'NONE',  ( -4.237492460401360996E-16, -1.000000000000000000, 0.000000000000000000 ) ) ;
#5645 = DIRECTION ( 'NONE',  ( 0.7071067811865517916, 0.000000000000000000, 0.7071067811865431318 ) ) ;
#5646 = ORIENTED_EDGE ( 'NONE', *, *, #4321, .T. ) ;
#5647 = DIRECTION ( 'NONE',  ( -1.000000000000000000, 4.270088556250607616E-16, -0.000000000000000000 ) ) ;
#5648 = CARTESIAN_POINT ( 'NONE',  ( 363.1933569832476678, 19.57388548866421019, -4.126530372600788255 ) ) ;
#5649 = VERTEX_POINT ( 'NONE', #6432 ) ;
#5650 = EDGE_CURVE ( 'NONE', #3493, #1999, #933, .T. ) ;
#5651 = CARTESIAN_POINT ( 'NONE',  ( 0.000000000000000000, 0.000000000000000000, 25.00000000000000000 ) ) ;
#5652 = ORIENTED_EDGE ( 'NONE', *, *, #2841, .T. ) ;
#5653 = PLANE ( 'NONE',  #4968 ) ;
#5654 = DIRECTION ( 'NONE',  ( 1.000000000000000000, 0.000000000000000000, -0.000000000000000000 ) ) ;
#5655 =( GEOMETRIC_REPRESENTATION_CONTEXT ( 3 ) GLOBAL_UNCERTAINTY_ASSIGNED_CONTEXT ( ( #6886 ) ) GLOBAL_UNIT_ASSIGNED_CONTEXT ( ( #1146, #7173, #7722 ) ) REPRESENTATION_CONTEXT ( 'NONE', 'WORKASPACE' ) );
#5656 = EDGE_LOOP ( 'NONE', ( #2276, #7092 ) ) ;
#5657 = ORIENTED_EDGE ( 'NONE', *, *, #4924, .F. ) ;
#5658 = ORIENTED_EDGE ( 'NONE', *, *, #85, .F. ) ;
#5659 = CARTESIAN_POINT ( 'NONE',  ( 333.3156402192583414, 150.0000000000000000, 178.7536863448640929 ) ) ;
#5660 = CARTESIAN_POINT ( 'NONE',  ( 380.6029633424947747, -16.57206429410149795, -11.20336317960804884 ) ) ;
#5661 = ORIENTED_EDGE ( 'NONE', *, *, #2484, .F. ) ;
#5662 = ORIENTED_EDGE ( 'NONE', *, *, #4883, .T. ) ;
#5663 = DIRECTION ( 'NONE',  ( -0.000000000000000000, -0.000000000000000000, -1.000000000000000000 ) ) ;
#5664 = ADVANCED_FACE ( 'NONE', ( #2059 ), #3430, .T. ) ;
#5665 = EDGE_CURVE ( 'NONE', #4997, #2860, #7594, .T. ) ;
#5666 = CARTESIAN_POINT ( 'NONE',  ( 326.6025403784438481, 150.0000000000000568, 125.0000000000000000 ) ) ;
#5667 = CARTESIAN_POINT ( 'NONE',  ( 15.00000000000000000, 0.000000000000000000, 47.50000000000000000 ) ) ;
#5668 = CARTESIAN_POINT ( 'NONE',  ( -31.24999999999997158, 177.4999999999999432, 130.0000000000000000 ) ) ;
#5669 = DIRECTION ( 'NONE',  ( 1.000000000000000000, 0.000000000000000000, 0.000000000000000000 ) ) ;
#5670 = EDGE_CURVE ( 'NONE', #2126, #7160, #3563, .T. ) ;
#5671 = EDGE_CURVE ( 'NONE', #5242, #2348, #7836, .T. ) ;
#5672 = ORIENTED_EDGE ( 'NONE', *, *, #1795, .T. ) ;
#5673 = B_SPLINE_CURVE_WITH_KNOTS ( 'NONE', 3,
 ( #462, #3382, #2219, #7711 ),
 .UNSPECIFIED., .F., .F.,
 ( 4, 4 ),
 ( 0.000000000000000000, 0.003328530869593415188 ),
 .UNSPECIFIED. ) ;
#5674 = CARTESIAN_POINT ( 'NONE',  ( 340.0000000000000000, -12.50000000000000355, -21.65063509461096558 ) ) ;
#5675 =( NAMED_UNIT ( * ) PLANE_ANGLE_UNIT ( ) SI_UNIT ( $, .RADIAN. ) );
#5676 = ORIENTED_EDGE ( 'NONE', *, *, #5324, .F. ) ;
#5677 = DIRECTION ( 'NONE',  ( -1.000000000000000000, -0.000000000000000000, -0.000000000000000000 ) ) ;
#5678 = FACE_OUTER_BOUND ( 'NONE', #3530, .T. ) ;
#5679 = CARTESIAN_POINT ( 'NONE',  ( -49.28095584970496645, 12.70544120911856112, 0.000000000000000000 ) ) ;
#5680 = CYLINDRICAL_SURFACE ( 'NONE', #6209, 5.000000000000000888 ) ;
#5681 = EDGE_LOOP ( 'NONE', ( #7384, #3152 ) ) ;
#5682 = EDGE_CURVE ( 'NONE', #7541, #5527, #1643, .T. ) ;
#5683 = VECTOR ( 'NONE', #1290, 1000.000000000000000 ) ;
#5684 = EDGE_LOOP ( 'NONE', ( #5319, #4200, #645, #5039 ) ) ;
#5685 = CARTESIAN_POINT ( 'NONE',  ( 367.3680131217492999, 17.37589182433591972, 9.907690019304302709 ) ) ;
#5686 = VERTEX_POINT ( 'NONE', #5425 ) ;
#5687 = DIRECTION ( 'NONE',  ( -0.000000000000000000, -0.000000000000000000, 1.000000000000000000 ) ) ;
#5689 = ORIENTED_EDGE ( 'NONE', *, *, #855, .F. ) ;
#5688 = AXIS2_PLACEMENT_3D ( 'NONE', #1969, #5548, #1413 ) ;
#5690 = VECTOR ( 'NONE', #1705, 1000.000000000000000 ) ;
#5691 = DIRECTION ( 'NONE',  ( 1.000000000000000000, 0.000000000000000000, 0.000000000000000000 ) ) ;
#5692 = DIRECTION ( 'NONE',  ( -0.000000000000000000, -0.000000000000000000, -1.000000000000000000 ) ) ;
#5693 = EDGE_CURVE ( 'NONE', #5607, #4926, #6073, .T. ) ;
#5694 = AXIS2_PLACEMENT_3D ( 'NONE', #1691, #6031, #3502 ) ;
#5695 = EDGE_LOOP ( 'NONE', ( #3951, #1913, #4202, #4838, #1799 ) ) ;
#5696 = LINE ( 'NONE', #2645, #7547 ) ;
#5697 = ORIENTED_EDGE ( 'NONE', *, *, #4894, .T. ) ;
#5698 = EDGE_LOOP ( 'NONE', ( #1624, #3087 ) ) ;
#5699 = FACE_OUTER_BOUND ( 'NONE', #5903, .T. ) ;
#5700 = CARTESIAN_POINT ( 'NONE',  ( 125.0000000000000000, 3.827021247335478902E-15, -31.25000000000000000 ) ) ;
#5701 = EDGE_LOOP ( 'NONE', ( #5141, #173, #1804, #3129 ) ) ;
#5702 = AXIS2_PLACEMENT_3D ( 'NONE', #966, #2693, #5159 ) ;
#5703 = AXIS2_PLACEMENT_3D ( 'NONE', #4620, #7717, #338 ) ;
#5704 = CYLINDRICAL_SURFACE ( 'NONE', #7233, 25.00000000000000711 ) ;
#5705 = CIRCLE ( 'NONE', #5958, 12.50000000000000000 ) ;
#5706 = AXIS2_PLACEMENT_3D ( 'NONE', #2502, #2541, #7472 ) ;
#5707 = AXIS2_PLACEMENT_3D ( 'NONE', #6583, #1690, #6465 ) ;
#5708 = CONTEXT_DEPENDENT_SHAPE_REPRESENTATION ( #6388, #3687 ) ;
#5709 = LINE ( 'NONE', #206, #5734 ) ;
#5710 = CARTESIAN_POINT ( 'NONE',  ( -25.00000000000000000, 0.000000000000000000, -25.00000000000000000 ) ) ;
#5711 = CARTESIAN_POINT ( 'NONE',  ( 375.0000000000000000, 15.61249499599599488, 12.50000000000000711 ) ) ;
#5712 = CARTESIAN_POINT ( 'NONE',  ( -25.00000000000000000, -25.00000000000000000, 50.00000000000000000 ) ) ;
#5713 = AXIS2_PLACEMENT_3D ( 'NONE', #3088, #6203, #6685 ) ;
#5714 = ORIENTED_EDGE ( 'NONE', *, *, #3316, .F. ) ;
#5715 = FACE_OUTER_BOUND ( 'NONE', #1096, .T. ) ;
#5716 = CIRCLE ( 'NONE', #4043, 12.50000000000000000 ) ;
#5717 = CARTESIAN_POINT ( 'NONE',  ( 303.6644303226191255, 194.6990734970208337, 230.9962291011739239 ) ) ;
#5718 = ORIENTED_EDGE ( 'NONE', *, *, #5380, .F. ) ;
#5719 = EDGE_CURVE ( 'NONE', #6900, #322, #2992, .T. ) ;
#5720 = CARTESIAN_POINT ( 'NONE',  ( 0.000000000000000000, 0.000000000000000000, 25.00000000000000000 ) ) ;
#5721 = CARTESIAN_POINT ( 'NONE',  ( 400.0000000000000568, 25.00000000000000000, 25.00000000000000000 ) ) ;
#5722 = CARTESIAN_POINT ( 'NONE',  ( 9.999999999999896971, 0.000000000000000000, 0.000000000000000000 ) ) ;
#5723 = DIRECTION ( 'NONE',  ( 1.000000000000000000, 0.000000000000000000, 0.000000000000000000 ) ) ;
#5724 = ORIENTED_EDGE ( 'NONE', *, *, #5671, .T. ) ;
#5725 = EDGE_CURVE ( 'NONE', #3485, #4601, #235, .T. ) ;
#5726 = ADVANCED_FACE ( 'NONE', ( #1137 ), #507, .T. ) ;
#5727 = DIRECTION ( 'NONE',  ( -1.000000000000000000, -0.000000000000000000, -0.000000000000000000 ) ) ;
#5728 = VERTEX_POINT ( 'NONE', #543 ) ;
#5729 = CARTESIAN_POINT ( 'NONE',  ( -27.49999999999989342, 187.4999999999999432, 12.50000000000000000 ) ) ;
#5730 = CIRCLE ( 'NONE', #2519, 4.999999999999997335 ) ;
#5731 = ORIENTED_EDGE ( 'NONE', *, *, #4828, .T. ) ;
#5732 = DIRECTION ( 'NONE',  ( -1.295260195396012743E-15, -1.000000000000000000, 0.000000000000000000 ) ) ;
#5733 = DIRECTION ( 'NONE',  ( -1.000000000000000000, 0.000000000000000000, 0.000000000000000000 ) ) ;
#5734 = VECTOR ( 'NONE', #46, 1000.000000000000000 ) ;
#5735 = VERTEX_POINT ( 'NONE', #2382 ) ;
#5736 = DIRECTION ( 'NONE',  ( -1.000000000000000000, 0.000000000000000000, 0.000000000000000000 ) ) ;
#5737 = EDGE_LOOP ( 'NONE', ( #7812, #111, #2232, #1686 ) ) ;
#5738 = ORIENTED_EDGE ( 'NONE', *, *, #5163, .T. ) ;
#5739 = CARTESIAN_POINT ( 'NONE',  ( -15.00000000000000000, 1.836970198721029589E-15, 47.50000000000000000 ) ) ;
#5740 = ADVANCED_FACE ( 'NONE', ( #7278 ), #5350, .T. ) ;
#5741 = FILL_AREA_STYLE ('',( #841 ) ) ;
#5743 = ORIENTED_EDGE ( 'NONE', *, *, #1587, .F. ) ;
#5742 = AXIS2_PLACEMENT_3D ( 'NONE', #1149, #5437, #6454 ) ;
#5744 = CYLINDRICAL_SURFACE ( 'NONE', #3390, 12.50000000000000355 ) ;
#5745 = AXIS2_PLACEMENT_3D ( 'NONE', #69, #4844, #2521 ) ;
#5746 = VECTOR ( 'NONE', #2746, 1000.000000000000000 ) ;
#5747 = VERTEX_POINT ( 'NONE', #4178 ) ;
#5748 = ITEM_DEFINED_TRANSFORMATION ( 'NONE', 'NONE', #5911,  #5785 ) ;
#5749 = LINE ( 'NONE', #3374, #1885 ) ;
#5750 = CARTESIAN_POINT ( 'NONE',  ( -74.28095588234631919, -62.29455879088143888, 12.50000000000000000 ) ) ;
#5751 = FACE_OUTER_BOUND ( 'NONE', #678, .T. ) ;
#5752 = DIRECTION ( 'NONE',  ( 1.000000000000000000, 0.000000000000000000, 0.000000000000000000 ) ) ;
#5753 = CIRCLE ( 'NONE', #4330, 12.50000000000000355 ) ;
#5754 = VECTOR ( 'NONE', #3187, 1000.000000000000000 ) ;
#5755 = ORIENTED_EDGE ( 'NONE', *, *, #735, .F. ) ;
#5756 = DIRECTION ( 'NONE',  ( 1.000000000000000000, 0.000000000000000000, 0.000000000000000000 ) ) ;
#5757 = AXIS2_PLACEMENT_3D ( 'NONE', #3244, #1214, #1255 ) ;
#5758 = AXIS2_PLACEMENT_3D ( 'NONE', #6510, #1013, #3465 ) ;
#5759 = ORIENTED_EDGE ( 'NONE', *, *, #6398, .T. ) ;
#5760 = CARTESIAN_POINT ( 'NONE',  ( 400.0000000000000568, 0.000000000000000000, 0.000000000000000000 ) ) ;
#5761 = LINE ( 'NONE', #1418, #6003 ) ;
#5762 = DIRECTION ( 'NONE',  ( 0.000000000000000000, -0.000000000000000000, 1.000000000000000000 ) ) ;
#5763 = DIRECTION ( 'NONE',  ( 0.000000000000000000, 0.000000000000000000, 1.000000000000000000 ) ) ;
#5764 = ORIENTED_EDGE ( 'NONE', *, *, #3825, .T. ) ;
#5765 = UNCERTAINTY_MEASURE_WITH_UNIT (LENGTH_MEASURE( 1.000000000000000082E-05 ), #1543, 'distance_accuracy_value', 'NONE');
#5766 = EDGE_CURVE ( 'NONE', #1635, #4483, #4778, .T. ) ;
#5767 = ORIENTED_EDGE ( 'NONE', *, *, #862, .T. ) ;
#5768 = ADVANCED_FACE ( 'NONE', ( #6673, #4819 ), #1056, .F. ) ;
#5769 = ORIENTED_EDGE ( 'NONE', *, *, #236, .T. ) ;
#5770 = FACE_BOUND ( 'NONE', #4522, .T. ) ;
#5771 = CARTESIAN_POINT ( 'NONE',  ( 175.0000000000000000, 0.000000000000000000, 0.000000000000000000 ) ) ;
#5772 = CARTESIAN_POINT ( 'NONE',  ( 0.000000000000000000, 0.000000000000000000, 77.49999999999998579 ) ) ;
#5773 = CARTESIAN_POINT ( 'NONE',  ( -1.301042606982605321E-15, -37.50000000000000000, 12.50000000000000000 ) ) ;
#5774 = EDGE_CURVE ( 'NONE', #30, #3534, #1618, .T. ) ;
#5775 =( REPRESENTATION_RELATIONSHIP ('NONE','NONE', #6292, #444 ) REPRESENTATION_RELATIONSHIP_WITH_TRANSFORMATION ( #4896 )SHAPE_REPRESENTATION_RELATIONSHIP( ) );
#5776 = ORIENTED_EDGE ( 'NONE', *, *, #4092, .F. ) ;
#5777 = DIRECTION ( 'NONE',  ( 0.000000000000000000, 0.000000000000000000, -1.000000000000000000 ) ) ;
#5778 = ORIENTED_EDGE ( 'NONE', *, *, #3338, .F. ) ;
#5779 = ORIENTED_EDGE ( 'NONE', *, *, #3666, .T. ) ;
#5780 = DIRECTION ( 'NONE',  ( 1.224646799147353207E-16, 1.000000000000000000, 0.000000000000000000 ) ) ;
#5781 = LINE ( 'NONE', #2728, #2495 ) ;
#5782 = DIRECTION ( 'NONE',  ( 0.000000000000000000, -1.000000000000000000, 0.000000000000000000 ) ) ;
#5783 = DIRECTION ( 'NONE',  ( 0.000000000000000000, 0.000000000000000000, -1.000000000000000000 ) ) ;
#5784 = EDGE_CURVE ( 'NONE', #5237, #2387, #6902, .T. ) ;
#5785 = AXIS2_PLACEMENT_3D ( 'NONE', #4110, #4186, #2351 ) ;
#5786 = VERTEX_POINT ( 'NONE', #2223 ) ;
#5787 = DIRECTION ( 'NONE',  ( -4.789677997474686366E-16, -1.000000000000000000, -0.000000000000000000 ) ) ;
#5788 = DIRECTION ( 'NONE',  ( -1.000000000000000000, 0.000000000000000000, 0.000000000000000000 ) ) ;
#5789 = CARTESIAN_POINT ( 'NONE',  ( 6.602357126051254174E-16, 0.000000000000000000, -31.78244274809162562 ) ) ;
#5790 = DIRECTION ( 'NONE',  ( -0.000000000000000000, -0.000000000000000000, -1.000000000000000000 ) ) ;
#5791 = CARTESIAN_POINT ( 'NONE',  ( -32.49999999999995026, 47.50000000000009237, 5.000000000000000000 ) ) ;
#5792 = CYLINDRICAL_SURFACE ( 'NONE', #709, 35.78244274809159720 ) ;
#5793 = EDGE_CURVE ( 'NONE', #6684, #2333, #1774, .T. ) ;
#5794 = CARTESIAN_POINT ( 'NONE',  ( -49.28095584970496645, -62.29455879088143888, 0.000000000000000000 ) ) ;
#5795 =( LENGTH_UNIT ( ) NAMED_UNIT ( * ) SI_UNIT ( .MILLI., .METRE. ) );
#5796 = ORIENTED_EDGE ( 'NONE', *, *, #2157, .F. ) ;
#5797 = PRESENTATION_STYLE_ASSIGNMENT (( #6395 ) ) ;
#5798 = CARTESIAN_POINT ( 'NONE',  ( 12.50000000000000355, 0.000000000000000000, 0.000000000000000000 ) ) ;
#5799 = DIRECTION ( 'NONE',  ( 1.295260195396012940E-15, 1.000000000000000000, 0.000000000000000000 ) ) ;
#5800 = DIRECTION ( 'NONE',  ( -1.000000000000000000, 0.000000000000000000, 0.000000000000000000 ) ) ;
#5801 = VERTEX_POINT ( 'NONE', #4064 ) ;
#5802 = ORIENTED_EDGE ( 'NONE', *, *, #3892, .T. ) ;
#5803 = CYLINDRICAL_SURFACE ( 'NONE', #7063, 25.00000000000002132 ) ;
#5804 = ORIENTED_EDGE ( 'NONE', *, *, #6686, .T. ) ;
#5805 = DIRECTION ( 'NONE',  ( -4.270088556250607616E-16, -1.000000000000000000, 0.000000000000000000 ) ) ;
#5806 = CARTESIAN_POINT ( 'NONE',  ( -26.24999999999997158, 177.6587708172406224, 12.50000000000000000 ) ) ;
#5807 = EDGE_CURVE ( 'NONE', #7780, #5649, #7800, .T. ) ;
#5808 = LINE ( 'NONE', #7646, #1722 ) ;
#5809 = ORIENTED_EDGE ( 'NONE', *, *, #724, .T. ) ;
#5810 = DIRECTION ( 'NONE',  ( -1.000000000000000000, 0.000000000000000000, 0.000000000000000000 ) ) ;
#5811 = EDGE_LOOP ( 'NONE', ( #5155, #379, #3058, #547 ) ) ;
#5812 = CIRCLE ( 'NONE', #2230, 12.50000000000000000 ) ;
#5813 = DIRECTION ( 'NONE',  ( 0.5000000000000001110, 0.8660254037844385966, 0.000000000000000000 ) ) ;
#5814 = EDGE_LOOP ( 'NONE', ( #6689, #4913 ) ) ;
#5815 = CYLINDRICAL_SURFACE ( 'NONE', #2660, 25.00000000000000000 ) ;
#5816 = EDGE_CURVE ( 'NONE', #443, #5938, #5223, .T. ) ;
#5817 = CARTESIAN_POINT ( 'NONE',  ( 340.0000000000000000, -12.50000000000000355, -15.61249499599599311 ) ) ;
#5818 = CARTESIAN_POINT ( 'NONE',  ( -49.28095584970496645, 12.70544120911856112, 12.50000000000000000 ) ) ;
#5819 = EDGE_CURVE ( 'NONE', #1396, #268, #2271, .T. ) ;
#5820 = AXIS2_PLACEMENT_3D ( 'NONE', #1025, #4065, #4820 ) ;
#5821 = ORIENTED_EDGE ( 'NONE', *, *, #3807, .T. ) ;
#5822 = EDGE_CURVE ( 'NONE', #387, #6174, #4139, .T. ) ;
#5823 = CIRCLE ( 'NONE', #7106, 25.00000000000000000 ) ;
#5824 = AXIS2_PLACEMENT_3D ( 'NONE', #6385, #6271, #3975 ) ;
#5825 = CARTESIAN_POINT ( 'NONE',  ( -10.49999999999999467, 1.408343819019455979E-15, 0.000000000000000000 ) ) ;
#5826 = DIRECTION ( 'NONE',  ( -1.000000000000000000, 4.270088556250607616E-16, 0.000000000000000000 ) ) ;
#5827 = CARTESIAN_POINT ( 'NONE',  ( -12.49999999999996803, 225.0000000000000284, 12.50000000000000000 ) ) ;
#5828 = CARTESIAN_POINT ( 'NONE',  ( 0.000000000000000000, -37.50000000000000000, 0.000000000000000000 ) ) ;
#5829 = CARTESIAN_POINT ( 'NONE',  ( 382.6415087606284828, 17.37175308249308969, 9.924386979199645964 ) ) ;
#5830 = TOROIDAL_SURFACE ( 'NONE', #6341, 12.50000000000000355, 5.000000000000000000 ) ;
#5831 = AXIS2_PLACEMENT_3D ( 'NONE', #2089, #4536, #7510 ) ;
#5832 = DIRECTION ( 'NONE',  ( 0.000000000000000000, 0.000000000000000000, 1.000000000000000000 ) ) ;
#5833 = VERTEX_POINT ( 'NONE', #1097 ) ;
#5834 = SURFACE_STYLE_FILL_AREA ( #3980 ) ;
#5835 = CARTESIAN_POINT ( 'NONE',  ( 12.50000000000000000, 1.530808498934191521E-15, 12.50000000000000000 ) ) ;
#5837 = DIRECTION ( 'NONE',  ( -1.000000000000000000, 0.000000000000000000, 0.000000000000000000 ) ) ;
#5836 = AXIS2_PLACEMENT_3D ( 'NONE', #2438, #3200, #707 ) ;
#5838 = EDGE_CURVE ( 'NONE', #2143, #4671, #7661, .T. ) ;
#5839 = CYLINDRICAL_SURFACE ( 'NONE', #5703, 12.50000000000001066 ) ;
#5840 = ORIENTED_EDGE ( 'NONE', *, *, #2533, .T. ) ;
#5841 = UNCERTAINTY_MEASURE_WITH_UNIT (LENGTH_MEASURE( 1.000000000000000082E-05 ), #1029, 'distance_accuracy_value', 'NONE');
#5842 = ORIENTED_EDGE ( 'NONE', *, *, #490, .T. ) ;
#5843 = ORIENTED_EDGE ( 'NONE', *, *, #3843, .T. ) ;
#5844 = CARTESIAN_POINT ( 'NONE',  ( 400.0000000000000568, 0.000000000000000000, 25.00000000000000000 ) ) ;
#5845 = ORIENTED_EDGE ( 'NONE', *, *, #6750, .T. ) ;
#5846 = CARTESIAN_POINT ( 'NONE',  ( 0.000000000000000000, 0.000000000000000000, 52.50000000000000000 ) ) ;
#5847 = ORIENTED_EDGE ( 'NONE', *, *, #5719, .F. ) ;
#5848 = AXIS2_PLACEMENT_3D ( 'NONE', #2798, #4074, #5234 ) ;
#5849 = FACE_BOUND ( 'NONE', #5890, .T. ) ;
#5850 = ORIENTED_EDGE ( 'NONE', *, *, #765, .F. ) ;
#5851 = VECTOR ( 'NONE', #5469, 1000.000000000000000 ) ;
#5852 = CARTESIAN_POINT ( 'NONE',  ( 0.000000000000000000, 0.000000000000000000, 0.000000000000000000 ) ) ;
#5853 = ORIENTED_EDGE ( 'NONE', *, *, #5936, .F. ) ;
#5854 = LINE ( 'NONE', #3366, #1355 ) ;
#5855 = ORIENTED_EDGE ( 'NONE', *, *, #3406, .T. ) ;
#5856 = DIRECTION ( 'NONE',  ( 0.000000000000000000, 0.000000000000000000, 1.000000000000000000 ) ) ;
#5857 = DIRECTION ( 'NONE',  ( 0.000000000000000000, 0.000000000000000000, -1.000000000000000000 ) ) ;
#5858 = CARTESIAN_POINT ( 'NONE',  ( 150.0000000000000000, 1.836970198721029747E-14, 25.00000000000000000 ) ) ;
#5859 = EDGE_CURVE ( 'NONE', #5409, #3124, #1132, .T. ) ;
#5860 = VERTEX_POINT ( 'NONE', #2500 ) ;
#5861 = CIRCLE ( 'NONE', #7149, 5.000000000000004441 ) ;
#5862 = EDGE_CURVE ( 'NONE', #2221, #3736, #2425, .T. ) ;
#5863 = DIRECTION ( 'NONE',  ( 0.000000000000000000, 1.000000000000000000, 0.000000000000000000 ) ) ;
#5864 = DIRECTION ( 'NONE',  ( 0.000000000000000000, 0.000000000000000000, 1.000000000000000000 ) ) ;
#5865 = DIRECTION ( 'NONE',  ( -1.000000000000000000, -0.000000000000000000, -0.000000000000000000 ) ) ;
#5866 = LINE ( 'NONE', #2091, #6966 ) ;
#5867 = CARTESIAN_POINT ( 'NONE',  ( 386.6668409306243461, 19.48969576164946105, 4.506197270647787967 ) ) ;
#5868 = CIRCLE ( 'NONE', #7302, 12.50000000000000000 ) ;
#5869 = CIRCLE ( 'NONE', #873, 12.50000000000000000 ) ;
#5870 = EDGE_CURVE ( 'NONE', #2527, #6578, #1930, .T. ) ;
#5871 = LINE ( 'NONE', #1732, #112 ) ;
#5872 = DIRECTION ( 'NONE',  ( -0.8593179320272661403, 4.115192332669971514E-16, -0.5114417774257230542 ) ) ;
#5873 = ORIENTED_EDGE ( 'NONE', *, *, #4090, .F. ) ;
#5874 = VECTOR ( 'NONE', #188, 1000.000000000000000 ) ;
#5875 = LINE ( 'NONE', #2270, #852 ) ;
#5876 = LINE ( 'NONE', #1541, #4196 ) ;
#5877 = CIRCLE ( 'NONE', #4978, 5.000000000000000888 ) ;
#5878 = DIRECTION ( 'NONE',  ( 0.000000000000000000, -1.000000000000000000, 0.000000000000000000 ) ) ;
#5879 = FACE_OUTER_BOUND ( 'NONE', #7131, .T. ) ;
#5880 = EDGE_LOOP ( 'NONE', ( #1104, #34, #6952, #170 ) ) ;
#5881 = VECTOR ( 'NONE', #239, 1000.000000000000114 ) ;
#5882 = ORIENTED_EDGE ( 'NONE', *, *, #5962, .F. ) ;
#5883 = AXIS2_PLACEMENT_3D ( 'NONE', #3023, #2454, #39 ) ;
#5884 = VERTEX_POINT ( 'NONE', #6872 ) ;
#5885 = EDGE_CURVE ( 'NONE', #1867, #1563, #7470, .T. ) ;
#5886 = ORIENTED_EDGE ( 'NONE', *, *, #1654, .T. ) ;
#5887 = DIRECTION ( 'NONE',  ( -0.000000000000000000, -0.000000000000000000, -1.000000000000000000 ) ) ;
#5888 = DIRECTION ( 'NONE',  ( 0.000000000000000000, 0.000000000000000000, 1.000000000000000000 ) ) ;
#5889 = AXIS2_PLACEMENT_3D ( 'NONE', #3566, #4717, #6014 ) ;
#5890 = EDGE_LOOP ( 'NONE', ( #5446, #3512 ) ) ;
#5891 = FACE_OUTER_BOUND ( 'NONE', #4510, .T. ) ;
#5892 = DIRECTION ( 'NONE',  ( 1.094506615593124353E-16, 1.000000000000000000, 0.000000000000000000 ) ) ;
#5893 = ADVANCED_FACE ( 'NONE', ( #7318 ), #4258, .T. ) ;
#5894 = DIRECTION ( 'NONE',  ( -1.000000000000000000, 0.000000000000000000, 0.000000000000000000 ) ) ;
#5895 = ORIENTED_EDGE ( 'NONE', *, *, #4143, .T. ) ;
#5896 = CARTESIAN_POINT ( 'NONE',  ( 199.9999999999998863, 225.0000000000000284, 0.000000000000000000 ) ) ;
#5897 = ORIENTED_EDGE ( 'NONE', *, *, #4053, .T. ) ;
#5898 = FACE_OUTER_BOUND ( 'NONE', #6349, .T. ) ;
#5899 = CARTESIAN_POINT ( 'NONE',  ( 0.000000000000000000, 0.000000000000000000, 0.000000000000000000 ) ) ;
#5900 = DIRECTION ( 'NONE',  ( -1.000000000000000000, -0.000000000000000000, -0.000000000000000000 ) ) ;
#5901 = CARTESIAN_POINT ( 'NONE',  ( -12.50000000000000000, -24.99999999999999645, -3.235013004037443297E-15 ) ) ;
#5902 = VERTEX_POINT ( 'NONE', #5591 ) ;
#5903 = EDGE_LOOP ( 'NONE', ( #4109, #6382, #660, #4441 ) ) ;
#5904 = DIRECTION ( 'NONE',  ( 0.000000000000000000, 0.000000000000000000, -1.000000000000000000 ) ) ;
#5905 = DIRECTION ( 'NONE',  ( -1.000000000000000000, 0.000000000000000000, 0.000000000000000000 ) ) ;
#5906 = CARTESIAN_POINT ( 'NONE',  ( -12.50000000000000000, 1.530808498934191521E-15, 12.50000000000000000 ) ) ;
#5907 = LINE ( 'NONE', #3422, #2610 ) ;
#5908 = EDGE_CURVE ( 'NONE', #150, #103, #6777, .T. ) ;
#5909 = DIRECTION ( 'NONE',  ( 0.000000000000000000, 0.000000000000000000, 1.000000000000000000 ) ) ;
#5910 = EDGE_CURVE ( 'NONE', #7209, #5922, #5546, .T. ) ;
#5911 = AXIS2_PLACEMENT_3D ( 'NONE', #7159, #378, #2827 ) ;
#5912 = LINE ( 'NONE', #4739, #5619 ) ;
#5913 = ORIENTED_EDGE ( 'NONE', *, *, #4950, .T. ) ;
#5914 = CARTESIAN_POINT ( 'NONE',  ( 0.000000000000000000, 0.000000000000000000, 0.5000000000000004441 ) ) ;
#5915 = DIRECTION ( 'NONE',  ( -1.000000000000000000, -0.000000000000000000, -0.000000000000000000 ) ) ;
#5916 = DIRECTION ( 'NONE',  ( 0.000000000000000000, 0.000000000000000000, -1.000000000000000000 ) ) ;
#5917 = EDGE_CURVE ( 'NONE', #6728, #3864, #6522, .T. ) ;
#5918 = ORIENTED_EDGE ( 'NONE', *, *, #5520, .T. ) ;
#5919 = ADVANCED_FACE ( 'NONE', ( #4298 ), #3149, .F. ) ;
#5920 = VERTEX_POINT ( 'NONE', #6828 ) ;
#5921 = ORIENTED_EDGE ( 'NONE', *, *, #4359, .T. ) ;
#5922 = VERTEX_POINT ( 'NONE', #47 ) ;
#5923 = EDGE_CURVE ( 'NONE', #5860, #6773, #1893, .T. ) ;
#5924 = DIRECTION ( 'NONE',  ( 1.000000000000000000, 0.000000000000000000, 0.000000000000000000 ) ) ;
#5925 = DIRECTION ( 'NONE',  ( -0.000000000000000000, 0.000000000000000000, 1.000000000000000000 ) ) ;
#5926 = ORIENTED_EDGE ( 'NONE', *, *, #567, .T. ) ;
#5927 = FILL_AREA_STYLE ('',( #3486 ) ) ;
#5928 = FACE_OUTER_BOUND ( 'NONE', #2995, .T. ) ;
#5929 = VERTEX_POINT ( 'NONE', #130 ) ;
#5930 = CARTESIAN_POINT ( 'NONE',  ( -8.959197987552832032, 23.33951095074251114, 25.00000000000000000 ) ) ;
#5931 = ORIENTED_EDGE ( 'NONE', *, *, #6185, .T. ) ;
#5932 = FACE_OUTER_BOUND ( 'NONE', #493, .T. ) ;
#5933 = EDGE_LOOP ( 'NONE', ( #1920, #1907, #5580, #529 ) ) ;
#5934 = DIRECTION ( 'NONE',  ( -0.000000000000000000, 0.000000000000000000, 1.000000000000000000 ) ) ;
#5935 = DIRECTION ( 'NONE',  ( -0.000000000000000000, -0.000000000000000000, -1.000000000000000000 ) ) ;
#5936 = EDGE_CURVE ( 'NONE', #3881, #6488, #628, .T. ) ;
#5937 = VECTOR ( 'NONE', #1560, 1000.000000000000000 ) ;
#5938 = VERTEX_POINT ( 'NONE', #3671 ) ;
#5939 = CIRCLE ( 'NONE', #3506, 12.50000000000000355 ) ;
#5940 = ORIENTED_EDGE ( 'NONE', *, *, #6711, .F. ) ;
#5941 = LINE ( 'NONE', #4853, #5080 ) ;
#5942 = CARTESIAN_POINT ( 'NONE',  ( 0.000000000000000000, 0.000000000000000000, 25.00000000000000000 ) ) ;
#5943 = CARTESIAN_POINT ( 'NONE',  ( 0.000000000000000000, 0.000000000000000000, 90.00000000000000000 ) ) ;
#5944 = CIRCLE ( 'NONE', #3514, 12.50000000000001066 ) ;
#5945 = AXIS2_PLACEMENT_3D ( 'NONE', #4347, #2434, #4868 ) ;
#5946 = CARTESIAN_POINT ( 'NONE',  ( -31.24999999999997158, 112.5000000000000142, 195.4980915752512658 ) ) ;
#5947 = DIRECTION ( 'NONE',  ( -0.000000000000000000, 0.000000000000000000, 1.000000000000000000 ) ) ;
#5948 = VECTOR ( 'NONE', #6619, 1000.000000000000000 ) ;
#5949 = CIRCLE ( 'NONE', #1335, 5.000000000000000888 ) ;
#5950 = CARTESIAN_POINT ( 'NONE',  ( 398.0000000000001137, -12.50000000000000000, 15.61249499599599488 ) ) ;
#5951 = PRODUCT_CONTEXT ( 'NONE', #4893, 'mechanical' ) ;
#5952 = ORIENTED_EDGE ( 'NONE', *, *, #3825, .F. ) ;
#5953 = CARTESIAN_POINT ( 'NONE',  ( 350.0000000000001137, -6.123233995736758985E-15, 25.00000000000000000 ) ) ;
#5954 = CARTESIAN_POINT ( 'NONE',  ( 296.6025403784437913, 82.50000000000004263, 155.0000000000000000 ) ) ;
#5955 = LINE ( 'NONE', #5351, #2362 ) ;
#5956 = DIRECTION ( 'NONE',  ( -0.000000000000000000, 0.000000000000000000, 1.000000000000000000 ) ) ;
#5957 = EDGE_LOOP ( 'NONE', ( #2410, #719, #3154, #935, #2792 ) ) ;
#5958 = AXIS2_PLACEMENT_3D ( 'NONE', #5532, #4281, #4922 ) ;
#5959 = TOROIDAL_SURFACE ( 'NONE', #3651, 12.50000000000000355, 5.000000000000000000 ) ;
#5960 = EDGE_LOOP ( 'NONE', ( #3641, #6808, #1835, #6126 ) ) ;
#5961 = VERTEX_POINT ( 'NONE', #1331 ) ;
#5962 = EDGE_CURVE ( 'NONE', #6439, #6900, #6257, .T. ) ;
#5963 = AXIS2_PLACEMENT_3D ( 'NONE', #4013, #1611, #7155 ) ;
#5964 =( NAMED_UNIT ( * ) PLANE_ANGLE_UNIT ( ) SI_UNIT ( $, .RADIAN. ) );
#5965 = EDGE_LOOP ( 'NONE', ( #5662, #7767 ) ) ;
#5966 = CARTESIAN_POINT ( 'NONE',  ( 296.6025403784437913, 142.5000000000000000, 155.0000000000000000 ) ) ;
#5967 = B_SPLINE_CURVE_WITH_KNOTS ( 'NONE', 3,
 ( #302, #2760, #7644, #2152 ),
 .UNSPECIFIED., .F., .F.,
 ( 4, 4 ),
 ( 0.000000000000000000, 0.001270006434950037748 ),
 .UNSPECIFIED. ) ;
#5968 = CYLINDRICAL_SURFACE ( 'NONE', #4392, 29.99999999999997158 ) ;
#5969 = EDGE_CURVE ( 'NONE', #7097, #5961, #5510, .T. ) ;
#5970 = ORIENTED_EDGE ( 'NONE', *, *, #251, .F. ) ;
#5971 = CARTESIAN_POINT ( 'NONE',  ( 158.9591979875528409, 23.33951095074252891, 0.000000000000000000 ) ) ;
#5972 = VECTOR ( 'NONE', #3321, 1000.000000000000000 ) ;
#5973 = EDGE_LOOP ( 'NONE', ( #7718, #1476, #2744, #1720 ) ) ;
#5974 = DIRECTION ( 'NONE',  ( -0.5000000000000002220, 0.8660254037844384856, 0.000000000000000000 ) ) ;
#5975 = ORIENTED_EDGE ( 'NONE', *, *, #6796, .F. ) ;
#5976 = DIRECTION ( 'NONE',  ( 0.000000000000000000, -0.000000000000000000, -1.000000000000000000 ) ) ;
#5977 = ORIENTED_EDGE ( 'NONE', *, *, #1589, .F. ) ;
#5978 = CARTESIAN_POINT ( 'NONE',  ( 398.0000000000001137, 0.000000000000000000, 0.000000000000000000 ) ) ;
#5979 = CARTESIAN_POINT ( 'NONE',  ( 398.0000000000001137, 0.000000000000000000, 0.000000000000000000 ) ) ;
#5980 = CIRCLE ( 'NONE', #2397, 12.50000000000001066 ) ;
#5981 = ORIENTED_EDGE ( 'NONE', *, *, #7522, .F. ) ;
#5982 = ORIENTED_EDGE ( 'NONE', *, *, #7821, .T. ) ;
#5983 = ADVANCED_FACE ( 'NONE', ( #2577 ), #732, .F. ) ;
#5984 = DIRECTION ( 'NONE',  ( 0.000000000000000000, 0.000000000000000000, 1.000000000000000000 ) ) ;
#5985 = CARTESIAN_POINT ( 'NONE',  ( 326.6025403784437913, 82.50000000000004263, 125.0000000000000000 ) ) ;
#5987 = CARTESIAN_POINT ( 'NONE',  ( 2.775557561562891351E-14, 225.0000000000000284, 12.50000000000000000 ) ) ;
#5986 = AXIS2_PLACEMENT_3D ( 'NONE', #6509, #1486, #2736 ) ;
#5988 = DIRECTION ( 'NONE',  ( -1.000000000000000000, 1.224646799147353454E-16, 0.000000000000000000 ) ) ;
#5989 = CARTESIAN_POINT ( 'NONE',  ( 381.3287739023131735, 16.83573837738345702, -10.80867071580873784 ) ) ;
#5990 = AXIS2_PLACEMENT_3D ( 'NONE', #7897, #1807, #2302 ) ;
#5991 = DIRECTION ( 'NONE',  ( 1.000000000000000000, -4.270088556250607616E-16, 0.000000000000000000 ) ) ;
#5992 = DIRECTION ( 'NONE',  ( -4.789152899817884163E-16, -0.9999999999999998890, 4.157528252923754350E-20 ) ) ;
#5993 = EDGE_LOOP ( 'NONE', ( #1948, #4781 ) ) ;
#5994 = CARTESIAN_POINT ( 'NONE',  ( 350.0000000000001137, -6.123233995736758985E-15, 25.00000000000000000 ) ) ;
#5995 = DIRECTION ( 'NONE',  ( 0.000000000000000000, -1.000000000000000000, 0.000000000000000000 ) ) ;
#5996 = CARTESIAN_POINT ( 'NONE',  ( 296.6025403784439050, 80.00000000000007105, 0.000000000000000000 ) ) ;
#5998 = EDGE_LOOP ( 'NONE', ( #5435, #823, #7038, #6841 ) ) ;
#5997 = AXIS2_PLACEMENT_3D ( 'NONE', #2895, #5934, #7221 ) ;
#5999 = VECTOR ( 'NONE', #6297, 1000.000000000000000 ) ;
#6000 = EDGE_CURVE ( 'NONE', #6519, #7538, #7033, .T. ) ;
#6001 = ORIENTED_EDGE ( 'NONE', *, *, #2988, .T. ) ;
#6002 = AXIS2_PLACEMENT_3D ( 'NONE', #7493, #2112, #870 ) ;
#6003 = VECTOR ( 'NONE', #3869, 1000.000000000000000 ) ;
#6004 = EDGE_LOOP ( 'NONE', ( #4159, #1531, #7329, #5567 ) ) ;
#6005 = CARTESIAN_POINT ( 'NONE',  ( 326.6025403784437913, 82.50000000000004263, 125.0000000000000000 ) ) ;
#6006 = CARTESIAN_POINT ( 'NONE',  ( -32.49999999999995026, 47.50000000000009237, 0.000000000000000000 ) ) ;
#6007 = ORIENTED_EDGE ( 'NONE', *, *, #2007, .T. ) ;
#6008 = CARTESIAN_POINT ( 'NONE',  ( 50.71904415029504065, 62.70544120911855401, 12.50000000000000000 ) ) ;
#6009 = CIRCLE ( 'NONE', #3073, 5.000000000000000000 ) ;
#6010 = ADVANCED_FACE ( 'NONE', ( #656 ), #7398, .F. ) ;
#6011 = AXIS2_PLACEMENT_3D ( 'NONE', #3375, #6426, #4452 ) ;
#6012 = EDGE_CURVE ( 'NONE', #2876, #1544, #1009, .T. ) ;
#6013 = ORIENTED_EDGE ( 'NONE', *, *, #2293, .T. ) ;
#6014 = DIRECTION ( 'NONE',  ( 1.000000000000000000, 0.000000000000000000, 0.000000000000000000 ) ) ;
#6015 = EDGE_LOOP ( 'NONE', ( #786, #1046, #4799, #3287, #4637 ) ) ;
#6016 = VECTOR ( 'NONE', #1636, 1000.000000000000000 ) ;
#6017 = CARTESIAN_POINT ( 'NONE',  ( 367.3650727329744541, -17.37719324208310923, -9.905392396107414399 ) ) ;
#6018 = AXIS2_PLACEMENT_3D ( 'NONE', #7193, #7269, #4129 ) ;
#6019 = EDGE_LOOP ( 'NONE', ( #4041, #1463, #247, #5622, #6939 ) ) ;
#6020 = CYLINDRICAL_SURFACE ( 'NONE', #2535, 12.50000000000000000 ) ;
#6021 = EDGE_CURVE ( 'NONE', #4246, #5251, #325, .T. ) ;
#6022 = LINE ( 'NONE', #527, #1220 ) ;
#6023 = EDGE_CURVE ( 'NONE', #2998, #5042, #2942, .T. ) ;
#6024 = EDGE_LOOP ( 'NONE', ( #1085, #7574, #4007, #5697 ) ) ;
#6025 = EDGE_LOOP ( 'NONE', ( #2287, #3594, #7823, #6960 ) ) ;
#6026 = CARTESIAN_POINT ( 'NONE',  ( 375.8509803977445927, -15.63011725355127624, 12.47807683047398619 ) ) ;
#6027 = PLANE ( 'NONE',  #3172 ) ;
#6028 = EDGE_CURVE ( 'NONE', #52, #869, #6343, .T. ) ;
#6029 = CARTESIAN_POINT ( 'NONE',  ( 400.0000000000000000, -12.50000000000000000, 25.00000000000000000 ) ) ;
#6030 = DIRECTION ( 'NONE',  ( 1.000000000000000000, 0.000000000000000000, 0.000000000000000000 ) ) ;
#6031 = DIRECTION ( 'NONE',  ( -1.000000000000000000, -0.000000000000000000, -0.000000000000000000 ) ) ;
#6032 = CARTESIAN_POINT ( 'NONE',  ( 386.6774787981661348, 19.49607926063143282, -4.478210459206754201 ) ) ;
#6033 = APPLICATION_CONTEXT ( 'automotive_design' ) ;
#6034 = DIRECTION ( 'NONE',  ( -1.000000000000000000, 0.000000000000000000, 0.000000000000000000 ) ) ;
#6035 = APPLICATION_PROTOCOL_DEFINITION ( 'draft international standard', 'automotive_design', 1998, #2748 ) ;
#6036 = DIRECTION ( 'NONE',  ( -1.000000000000000000, -0.000000000000000000, -0.000000000000000000 ) ) ;
#6037 = DIRECTION ( 'NONE',  ( 1.000000000000000000, 0.000000000000000000, 0.000000000000000000 ) ) ;
#6038 = PLANE ( 'NONE',  #7861 ) ;
#6039 = CARTESIAN_POINT ( 'NONE',  ( 199.9999999999998863, 225.0000000000000284, 12.50000000000000000 ) ) ;
#6040 = ORIENTED_EDGE ( 'NONE', *, *, #6839, .T. ) ;
#6041 = EDGE_CURVE ( 'NONE', #2004, #5012, #5877, .T. ) ;
#6042 = EDGE_LOOP ( 'NONE', ( #3354, #5843, #1879, #355 ) ) ;
#6043 = ORIENTED_EDGE ( 'NONE', *, *, #2255, .F. ) ;
#6044 = VERTEX_POINT ( 'NONE', #6948 ) ;
#6045 = LINE ( 'NONE', #7738, #2536 ) ;
#6046 = DIRECTION ( 'NONE',  ( 0.000000000000000000, 0.000000000000000000, 1.000000000000000000 ) ) ;
#6047 = AXIS2_PLACEMENT_3D ( 'NONE', #3305, #6919, #3866 ) ;
#6048 = DIRECTION ( 'NONE',  ( 0.000000000000000000, 0.000000000000000000, 1.000000000000000000 ) ) ;
#6049 = ORIENTED_EDGE ( 'NONE', *, *, #6445, .F. ) ;
#6050 = DIRECTION ( 'NONE',  ( -1.000000000000000000, 0.000000000000000000, 0.000000000000000000 ) ) ;
#6051 = PRODUCT_DEFINITION_SHAPE ( 'NONE', 'NONE',  #7932 ) ;
#6052 = CARTESIAN_POINT ( 'NONE',  ( 335.4891275541129971, 82.50000000000004263, 174.3961449365926626 ) ) ;
#6053 = ORIENTED_EDGE ( 'NONE', *, *, #4395, .F. ) ;
#6054 = CARTESIAN_POINT ( 'NONE',  ( 365.6270046772841624, -18.20868245435311295, 8.279865652961362343 ) ) ;
#6055 = EDGE_LOOP ( 'NONE', ( #1460, #2171 ) ) ;
#6056 = CARTESIAN_POINT ( 'NONE',  ( 0.7190441502950353225, 62.70544120911855401, 0.000000000000000000 ) ) ;
#6057 = DIRECTION ( 'NONE',  ( -1.000000000000000000, -0.000000000000000000, -0.000000000000000000 ) ) ;
#6058 = ORIENTED_EDGE ( 'NONE', *, *, #3226, .T. ) ;
#6059 = ORIENTED_EDGE ( 'NONE', *, *, #7449, .T. ) ;
#6060 = VECTOR ( 'NONE', #5626, 1000.000000000000000 ) ;
#6061 = EDGE_CURVE ( 'NONE', #5349, #4036, #2419, .T. ) ;
#6062 = DIRECTION ( 'NONE',  ( -1.000000000000000000, -0.000000000000000000, -0.000000000000000000 ) ) ;
#6063 = CARTESIAN_POINT ( 'NONE',  ( 50.71904415029504065, 62.70544120911855401, 12.50000000000000000 ) ) ;
#6064 = CARTESIAN_POINT ( 'NONE',  ( 0.000000000000000000, 0.000000000000000000, 25.00000000000000000 ) ) ;
#6065 = CARTESIAN_POINT ( 'NONE',  ( -26.24999999999997158, 0.000000000000000000, 17.50000000000001421 ) ) ;
#6066 = ADVANCED_FACE ( 'NONE', ( #7623, #2173 ), #2657, .F. ) ;
#6067 = DIRECTION ( 'NONE',  ( -0.000000000000000000, -0.000000000000000000, -1.000000000000000000 ) ) ;
#6068 = LINE ( 'NONE', #3026, #7875 ) ;
#6069 = CYLINDRICAL_SURFACE ( 'NONE', #3953, 17.50000000000000355 ) ;
#6070 = VECTOR ( 'NONE', #693, 1000.000000000000000 ) ;
#6071 = APPLICATION_PROTOCOL_DEFINITION ( 'draft international standard', 'automotive_design', 1998, #2184 ) ;
#6072 = CARTESIAN_POINT ( 'NONE',  ( 286.6025403784437913, 150.0000000000000284, 12.50000000000000000 ) ) ;
#6073 = LINE ( 'NONE', #7868, #2668 ) ;
#6074 = DIRECTION ( 'NONE',  ( -0.000000000000000000, 0.000000000000000000, -1.000000000000000000 ) ) ;
#6075 = LINE ( 'NONE', #6155, #1723 ) ;
#6076 = EDGE_CURVE ( 'NONE', #3451, #646, #2778, .T. ) ;
#6077 = AXIS2_PLACEMENT_3D ( 'NONE', #5417, #7350, #7902 ) ;
#6078 = VECTOR ( 'NONE', #4584, 1000.000000000000000 ) ;
#6079 = ORIENTED_EDGE ( 'NONE', *, *, #5671, .F. ) ;
#6080 = ORIENTED_EDGE ( 'NONE', *, *, #2685, .T. ) ;
#6081 = ADVANCED_FACE ( 'NONE', ( #1411 ), #3070, .T. ) ;
#6082 =( NAMED_UNIT ( * ) SI_UNIT ( $, .STERADIAN. ) SOLID_ANGLE_UNIT ( ) );
#6083 = DIRECTION ( 'NONE',  ( 1.000000000000000000, 0.000000000000000000, 0.000000000000000000 ) ) ;
#6084 = LINE ( 'NONE', #1106, #4776 ) ;
#6085=STYLED_ITEM('',(#7976),#1743);
#6086 = AXIS2_PLACEMENT_3D ( 'NONE', #5471, #6074, #4941 ) ;
#6087 = SURFACE_SIDE_STYLE ('',( #4908 ) ) ;
#6088 = VERTEX_POINT ( 'NONE', #2129 ) ;
#6089 = DIRECTION ( 'NONE',  ( 0.4463453945640545317, 0.000000000000000000, -0.8948607650084221543 ) ) ;
#6090 = CIRCLE ( 'NONE', #3272, 5.000000000000004441 ) ;
#6091 = ORIENTED_EDGE ( 'NONE', *, *, #5923, .F. ) ;
#6092 = CIRCLE ( 'NONE', #2628, 25.00000000000000000 ) ;
#6093 = CARTESIAN_POINT ( 'NONE',  ( 12.50000000000000000, 0.000000000000000000, 31.24999999999998579 ) ) ;
#6094 = ORIENTED_EDGE ( 'NONE', *, *, #7332, .F. ) ;
#6095 = CARTESIAN_POINT ( 'NONE',  ( 371.6755651776492186, -15.95794361973645792, -12.05683462702026176 ) ) ;
#6096 = ORIENTED_EDGE ( 'NONE', *, *, #1374, .F. ) ;
#6097 = CARTESIAN_POINT ( 'NONE',  ( -66.45428044951677293, 30.87346046883880035, 12.50000000000000000 ) ) ;
#6098 = AXIS2_PLACEMENT_3D ( 'NONE', #1826, #4998, #6089 ) ;
#6099 = FACE_OUTER_BOUND ( 'NONE', #1876, .T. ) ;
#6100 = ORIENTED_EDGE ( 'NONE', *, *, #2937, .T. ) ;
#6101 = AXIS2_PLACEMENT_3D ( 'NONE', #2638, #151, #1947 ) ;
#6102 = VERTEX_POINT ( 'NONE', #4570 ) ;
#6103 = DIRECTION ( 'NONE',  ( -1.000000000000000000, -0.000000000000000000, -0.000000000000000000 ) ) ;
#6104 = CARTESIAN_POINT ( 'NONE',  ( 158.9591979875528409, 23.33951095074252891, 0.000000000000000000 ) ) ;
#6105 = DIRECTION ( 'NONE',  ( 0.5000000000000001110, -0.8660254037844385966, 0.000000000000000000 ) ) ;
#6106 = CYLINDRICAL_SURFACE ( 'NONE', #3122, 5.000000000000000888 ) ;
#6107 = CARTESIAN_POINT ( 'NONE',  ( 75.00000000000000000, 55.56842436860067380, 0.000000000000000000 ) ) ;
#6108 = VECTOR ( 'NONE', #4669, 1000.000000000000000 ) ;
#6109 = CARTESIAN_POINT ( 'NONE',  ( 384.3951573019774628, 18.21476284106545052, -8.283543559714008353 ) ) ;
#6110 = ADVANCED_FACE ( 'NONE', ( #3861 ), #7068, .F. ) ;
#6111 = EDGE_CURVE ( 'NONE', #7342, #6165, #806, .T. ) ;
#6112 = CARTESIAN_POINT ( 'NONE',  ( -18.76388374866283471, 7.854341805648601650E-17, 7.500000000000000000 ) ) ;
#6113 =( GEOMETRIC_REPRESENTATION_CONTEXT ( 3 ) GLOBAL_UNCERTAINTY_ASSIGNED_CONTEXT ( ( #1506 ) ) GLOBAL_UNIT_ASSIGNED_CONTEXT ( ( #4897, #1663, #1698 ) ) REPRESENTATION_CONTEXT ( 'NONE', 'WORKASPACE' ) );
#6114 = ITEM_DEFINED_TRANSFORMATION ( 'NONE', 'NONE', #5399,  #5785 ) ;
#6115 = DIRECTION ( 'NONE',  ( 1.000000000000000000, 0.000000000000000000, 0.000000000000000000 ) ) ;
#6116 = DIRECTION ( 'NONE',  ( 1.000000000000000000, 0.000000000000000000, 0.000000000000000000 ) ) ;
#6117 = CYLINDRICAL_SURFACE ( 'NONE', #5422, 12.50000000000001066 ) ;
#6118 = EDGE_CURVE ( 'NONE', #3644, #7342, #4715, .T. ) ;
#6119 = ORIENTED_EDGE ( 'NONE', *, *, #3220, .F. ) ;
#6120 = ORIENTED_EDGE ( 'NONE', *, *, #5822, .F. ) ;
#6121 = FILL_AREA_STYLE_COLOUR ( '', #7889 ) ;
#6122 = DIRECTION ( 'NONE',  ( -4.237492460401359023E-16, -1.000000000000000000, 0.000000000000000000 ) ) ;
#6123 = AXIS2_PLACEMENT_3D ( 'NONE', #1788, #5201, #4830 ) ;
#6124 = CARTESIAN_POINT ( 'NONE',  ( -49.28095584970496645, 12.70544120911856112, 12.50000000000000000 ) ) ;
#6125 = CARTESIAN_POINT ( 'NONE',  ( 286.6025403784439050, 90.00000000000001421, 12.50000000000000000 ) ) ;
#6126 = ORIENTED_EDGE ( 'NONE', *, *, #6363, .F. ) ;
#6127 = CARTESIAN_POINT ( 'NONE',  ( -12.50000000000000000, 0.000000000000000000, 1.000000000000028644 ) ) ;
#6128 = CIRCLE ( 'NONE', #758, 18.00000000000007105 ) ;
#6129 = AXIS2_PLACEMENT_3D ( 'NONE', #2955, #6558, #3589 ) ;
#6130 = CARTESIAN_POINT ( 'NONE',  ( 370.8878672368923048, 16.14034269873396710, 11.81156333678811876 ) ) ;
#6131 = ORIENTED_EDGE ( 'NONE', *, *, #4334, .F. ) ;
#6132 = CARTESIAN_POINT ( 'NONE',  ( 370.5028268974027696, -16.24331487217730796, -11.67016537472322746 ) ) ;
#6133 = EDGE_LOOP ( 'NONE', ( #6394, #1423, #7146, #6714 ) ) ;
#6134 = PRESENTATION_LAYER_ASSIGNMENT (  '', '', ( #7660 ) ) ;
#6135 = CARTESIAN_POINT ( 'NONE',  ( -27.49999999999994671, 47.50000000000009237, 12.50000000000000000 ) ) ;
#6136 = AXIS2_PLACEMENT_3D ( 'NONE', #5209, #2088, #3895 ) ;
#6137 = FACE_BOUND ( 'NONE', #1225, .T. ) ;
#6138 = ADVANCED_FACE ( 'NONE', ( #3256 ), #3576, .T. ) ;
#6139 = ORIENTED_EDGE ( 'NONE', *, *, #7439, .T. ) ;
#6140 = AXIS2_PLACEMENT_3D ( 'NONE', #7834, #2866, #7672 ) ;
#6141 = VECTOR ( 'NONE', #1607, 1000.000000000000000 ) ;
#6142 = ORIENTED_EDGE ( 'NONE', *, *, #7821, .F. ) ;
#6143 = ORIENTED_EDGE ( 'NONE', *, *, #7391, .T. ) ;
#6144 = DIRECTION ( 'NONE',  ( 0.4463453945640545317, 0.000000000000000000, -0.8948607650084221543 ) ) ;
#6145 = CARTESIAN_POINT ( 'NONE',  ( -13.00000000000000178, 1.592040838891559293E-15, 2.168404344971008868E-16 ) ) ;
#6146 = DIRECTION ( 'NONE',  ( 0.000000000000000000, 0.000000000000000000, 1.000000000000000000 ) ) ;
#6147 = CYLINDRICAL_SURFACE ( 'NONE', #5537, 25.00000000000000711 ) ;
#6148 = CARTESIAN_POINT ( 'NONE',  ( 46.25000000000002842, 111.9999999999999858, 130.0000000000000000 ) ) ;
#6149 = CARTESIAN_POINT ( 'NONE',  ( 400.0000000000000568, 0.000000000000000000, 25.00000000000000000 ) ) ;
#6150 = APPLICATION_PROTOCOL_DEFINITION ( 'draft international standard', 'automotive_design', 1998, #6650 ) ;
#6151 = EDGE_CURVE ( 'NONE', #3922, #4349, #1566, .T. ) ;
#6152 = CARTESIAN_POINT ( 'NONE',  ( 325.0000000000000000, -12.50000000000000000, 21.65063509461096913 ) ) ;
#6153 = DIRECTION ( 'NONE',  ( 0.000000000000000000, 1.000000000000000000, 0.000000000000000000 ) ) ;
#6154 = CARTESIAN_POINT ( 'NONE',  ( 0.000000000000000000, 0.000000000000000000, 82.49999999999998579 ) ) ;
#6155 = CARTESIAN_POINT ( 'NONE',  ( 212.4999999999999147, 225.0000000000000284, 12.50000000000000000 ) ) ;
#6156 = ADVANCED_FACE ( 'NONE', ( #6270 ), #889, .F. ) ;
#6157 = ORIENTED_EDGE ( 'NONE', *, *, #2675, .F. ) ;
#6158 = EDGE_CURVE ( 'NONE', #4115, #150, #3936, .T. ) ;
#6159 = ORIENTED_EDGE ( 'NONE', *, *, #420, .T. ) ;
#6160 = EDGE_CURVE ( 'NONE', #5938, #7303, #1530, .T. ) ;
#6161 = CARTESIAN_POINT ( 'NONE',  ( 350.0000000000001137, -6.123233995736758985E-15, 0.000000000000000000 ) ) ;
#6162 = CARTESIAN_POINT ( 'NONE',  ( 232.4759526419164786, -18.74999999999998934, 12.50000000000000000 ) ) ;
#6163 = CARTESIAN_POINT ( 'NONE',  ( -24.28095581706362083, -62.29455879088143888, 0.000000000000000000 ) ) ;
#6164 = PLANE ( 'NONE',  #1334 ) ;
#6165 = VERTEX_POINT ( 'NONE', #2303 ) ;
#6166 = ADVANCED_FACE ( 'NONE', ( #4170 ), #1127, .T. ) ;
#6167 = DIRECTION ( 'NONE',  ( 0.000000000000000000, 0.000000000000000000, 1.000000000000000000 ) ) ;
#6168 = ORIENTED_EDGE ( 'NONE', *, *, #1741, .T. ) ;
#6169 = EDGE_CURVE ( 'NONE', #5516, #7370, #1726, .T. ) ;
#6170 = CARTESIAN_POINT ( 'NONE',  ( 370.5038504081379642, 16.24311277381278984, 11.67040959636601016 ) ) ;
#6172 = ORIENTED_EDGE ( 'NONE', *, *, #3921, .F. ) ;
#6171 = PRODUCT_DEFINITION_FORMATION_WITH_SPECIFIED_SOURCE ( 'ANY', '', #1621, .NOT_KNOWN. ) ;
#6173 = CARTESIAN_POINT ( 'NONE',  ( 362.5817914570322387, -19.94855572367474750, -1.655112461855906769 ) ) ;
#6174 = VERTEX_POINT ( 'NONE', #5415 ) ;
#6175 = DIRECTION ( 'NONE',  ( 1.094506615593124353E-16, 1.000000000000000000, 0.000000000000000000 ) ) ;
#6176 = CARTESIAN_POINT ( 'NONE',  ( -12.50000000000000000, 1.530808498934191521E-15, 2.000000000000001776 ) ) ;
#6177 = EDGE_CURVE ( 'NONE', #7492, #2860, #2373, .T. ) ;
#6178 = ORIENTED_EDGE ( 'NONE', *, *, #928, .T. ) ;
#6179 = VERTEX_POINT ( 'NONE', #412 ) ;
#6180 = SHAPE_REPRESENTATION ( 'Joint Plane', ( #5785 ), #3097 ) ;
#6181 = ORIENTED_EDGE ( 'NONE', *, *, #6207, .F. ) ;
#6182 = APPLICATION_CONTEXT ( 'automotive_design' ) ;
#6183 = CARTESIAN_POINT ( 'NONE',  ( 379.4961495918622632, -16.24311277381278984, 11.67040959636601016 ) ) ;
#6184 = CIRCLE ( 'NONE', #3996, 17.50000000000000355 ) ;
#6185 = EDGE_CURVE ( 'NONE', #1064, #1390, #6267, .T. ) ;
#6186 = CARTESIAN_POINT ( 'NONE',  ( -34.37499999999996447, 112.5000000000000142, 195.4980915752512658 ) ) ;
#6187 = DIRECTION ( 'NONE',  ( 0.000000000000000000, 0.000000000000000000, -1.000000000000000000 ) ) ;
#6188 = DIRECTION ( 'NONE',  ( 0.000000000000000000, 1.000000000000000000, 0.000000000000000000 ) ) ;
#6189 = DIRECTION ( 'NONE',  ( -0.000000000000000000, -0.000000000000000000, -1.000000000000000000 ) ) ;
#6190 = CONTEXT_DEPENDENT_SHAPE_REPRESENTATION ( #4333, #1687 ) ;
#6191 = FACE_OUTER_BOUND ( 'NONE', #4706, .T. ) ;
#6192 = DIRECTION ( 'NONE',  ( 0.000000000000000000, 1.000000000000000000, 0.000000000000000000 ) ) ;
#6193 = LINE ( 'NONE', #1968, #449 ) ;
#6194 = FACE_BOUND ( 'NONE', #7648, .T. ) ;
#6195 = ORIENTED_EDGE ( 'NONE', *, *, #3412, .F. ) ;
#6196 = AXIS2_PLACEMENT_3D ( 'NONE', #989, #1549, #3400 ) ;
#6197 = ORIENTED_EDGE ( 'NONE', *, *, #1980, .F. ) ;
#6198 = DIRECTION ( 'NONE',  ( 0.000000000000000000, -0.000000000000000000, 1.000000000000000000 ) ) ;
#6199 = CYLINDRICAL_SURFACE ( 'NONE', #7657, 24.99999996734539920 ) ;
#6200 = CARTESIAN_POINT ( 'NONE',  ( 10.82531754730548279, -13.74999999999999645, 7.500000000000000000 ) ) ;
#6201 = CARTESIAN_POINT ( 'NONE',  ( 17.32050807568877104, -2.500000000000002220, 7.500000000000000000 ) ) ;
#6202 = ORIENTED_EDGE ( 'NONE', *, *, #7618, .T. ) ;
#6203 = DIRECTION ( 'NONE',  ( 0.000000000000000000, -0.000000000000000000, -1.000000000000000000 ) ) ;
#6204 = AXIS2_PLACEMENT_3D ( 'NONE', #337, #6317, #5799 ) ;
#6205 = ADVANCED_FACE ( 'NONE', ( #4732 ), #4809, .T. ) ;
#6206 = VECTOR ( 'NONE', #844, 1000.000000000000000 ) ;
#6207 = EDGE_CURVE ( 'NONE', #7894, #4997, #368, .T. ) ;
#6208 = CARTESIAN_POINT ( 'NONE',  ( 367.3565110264916029, 17.37246880845878039, -9.923319895790875478 ) ) ;
#6209 = AXIS2_PLACEMENT_3D ( 'NONE', #7519, #2629, #6959 ) ;
#6210 = EDGE_LOOP ( 'NONE', ( #5089, #5206, #474, #4000 ) ) ;
#6211 = AXIS2_PLACEMENT_3D ( 'NONE', #2578, #3673, #6231 ) ;
#6212 = CARTESIAN_POINT ( 'NONE',  ( 17.32050807568877104, 2.500000000000000444, 7.500000000000000000 ) ) ;
#6213 = ORIENTED_EDGE ( 'NONE', *, *, #2793, .T. ) ;
#6214 = CARTESIAN_POINT ( 'NONE',  ( 0.000000000000000000, 0.000000000000000000, 25.00000000000000000 ) ) ;
#6215 = AXIS2_PLACEMENT_3D ( 'NONE', #5376, #7822, #4763 ) ;
#6216 = AXIS2_PLACEMENT_3D ( 'NONE', #1372, #3822, #4340 ) ;
#6217 = CIRCLE ( 'NONE', #5575, 5.000000000000000888 ) ;
#6218 = ORIENTED_EDGE ( 'NONE', *, *, #1863, .F. ) ;
#6219 = EDGE_LOOP ( 'NONE', ( #5718, #6447, #7074, #3516, #2289, #5672, #5198, #6436, #4127, #3203, #143, #2193 ) ) ;
#6220 = VECTOR ( 'NONE', #1051, 1000.000000000000227 ) ;
#6221 = ORIENTED_EDGE ( 'NONE', *, *, #6916, .T. ) ;
#6222 = CARTESIAN_POINT ( 'NONE',  ( 296.6025403784439050, 80.00000000000007105, 0.000000000000000000 ) ) ;
#6223 = DIRECTION ( 'NONE',  ( 1.000000000000000000, 0.000000000000000000, -0.000000000000000000 ) ) ;
#6224 = CARTESIAN_POINT ( 'NONE',  ( -27.49999999999994671, 42.50000000000009237, 0.000000000000000000 ) ) ;
#6225 = CARTESIAN_POINT ( 'NONE',  ( 0.000000000000000000, 3.061616997868383043E-15, -25.00000000000000000 ) ) ;
#6226 = LINE ( 'NONE', #6788, #6588 ) ;
#6227 = AXIS2_PLACEMENT_3D ( 'NONE', #7528, #4355, #6929 ) ;
#6228 = ADVANCED_FACE ( 'NONE', ( #7227 ), #5372, .F. ) ;
#6229 = DIRECTION ( 'NONE',  ( 1.000000000000000000, 0.000000000000000000, -0.000000000000000000 ) ) ;
#6230 = CARTESIAN_POINT ( 'NONE',  ( 0.000000000000000000, 0.000000000000000000, 82.49999999999998579 ) ) ;
#6231 = DIRECTION ( 'NONE',  ( 1.000000000000000000, 0.000000000000000000, -0.000000000000000000 ) ) ;
#6232 = LINE ( 'NONE', #5712, #4649 ) ;
#6233 = ORIENTED_EDGE ( 'NONE', *, *, #4920, .F. ) ;
#6234 = VECTOR ( 'NONE', #5179, 1000.000000000000000 ) ;
#6235 = ORIENTED_EDGE ( 'NONE', *, *, #1766, .T. ) ;
#6236 = DIRECTION ( 'NONE',  ( 0.000000000000000000, 0.000000000000000000, -1.000000000000000000 ) ) ;
#6237 = LINE ( 'NONE', #631, #5487 ) ;
#6238 = DIRECTION ( 'NONE',  ( -1.000000000000000000, 4.270088556250607616E-16, 0.000000000000000000 ) ) ;
#6239 = DIRECTION ( 'NONE',  ( -1.000000000000000000, -0.000000000000000000, -0.000000000000000000 ) ) ;
#6240 = VERTEX_POINT ( 'NONE', #5382 ) ;
#6241 = AXIS2_PLACEMENT_3D ( 'NONE', #3618, #2861, #5294 ) ;
#6242 = DIRECTION ( 'NONE',  ( -0.8886649088774989380, 0.4585571717133496983, 0.000000000000000000 ) ) ;
#6243 = EDGE_LOOP ( 'NONE', ( #5714, #518, #3926, #711 ) ) ;
#6244 = AXIS2_PLACEMENT_3D ( 'NONE', #959, #3040, #4003 ) ;
#6245 = CARTESIAN_POINT ( 'NONE',  ( 340.0000000000000000, 0.000000000000000000, 0.000000000000000000 ) ) ;
#6246 = EDGE_LOOP ( 'NONE', ( #5873, #6859, #4746, #2038, #1422, #5353, #5522, #215 ) ) ;
#6247 = CARTESIAN_POINT ( 'NONE',  ( 0.000000000000000000, 0.000000000000000000, 7.500000000000000000 ) ) ;
#6248 = ORIENTED_EDGE ( 'NONE', *, *, #4293, .T. ) ;
#6249 = EDGE_CURVE ( 'NONE', #3234, #2065, #637, .T. ) ;
#6250 = CARTESIAN_POINT ( 'NONE',  ( -37.50000000000000000, 4.857225732735047243E-14, 0.000000000000000000 ) ) ;
#6251 = CARTESIAN_POINT ( 'NONE',  ( 339.1025403784437913, 75.00000000000005684, 125.0000000000000000 ) ) ;
#6252 = CIRCLE ( 'NONE', #495, 12.49999999999999467 ) ;
#6253 = EDGE_CURVE ( 'NONE', #3485, #4076, #7707, .T. ) ;
#6254 = VERTEX_POINT ( 'NONE', #7752 ) ;
#6255 = ORIENTED_EDGE ( 'NONE', *, *, #6670, .F. ) ;
#6256 = VECTOR ( 'NONE', #2662, 1000.000000000000000 ) ;
#6257 = CIRCLE ( 'NONE', #508, 25.00000000000000000 ) ;
#6258 = EDGE_CURVE ( 'NONE', #4433, #4036, #4647, .T. ) ;
#6259 = VERTEX_POINT ( 'NONE', #4055 ) ;
#6260 = LINE ( 'NONE', #5659, #3940 ) ;
#6261 = EDGE_CURVE ( 'NONE', #260, #3577, #3960, .T. ) ;
#6262 = DIRECTION ( 'NONE',  ( 0.000000000000000000, 1.000000000000000000, -0.000000000000000000 ) ) ;
#6263 = DIRECTION ( 'NONE',  ( 1.000000000000000000, 2.960594732333750117E-15, -0.000000000000000000 ) ) ;
#6264 = VERTEX_POINT ( 'NONE', #2260 ) ;
#6265 = DIRECTION ( 'NONE',  ( -1.000000000000000000, -0.000000000000000000, -0.000000000000000000 ) ) ;
#6266 = AXIS2_PLACEMENT_3D ( 'NONE', #2826, #5260, #5832 ) ;
#6267 = CIRCLE ( 'NONE', #6018, 12.50000000000000000 ) ;
#6268 = AXIS2_PLACEMENT_3D ( 'NONE', #4081, #6538, #3490 ) ;
#6269 = CYLINDRICAL_SURFACE ( 'NONE', #1113, 12.50000000000001066 ) ;
#6270 = FACE_OUTER_BOUND ( 'NONE', #6986, .T. ) ;
#6271 = DIRECTION ( 'NONE',  ( -0.000000000000000000, -0.000000000000000000, -1.000000000000000000 ) ) ;
#6272 = DIRECTION ( 'NONE',  ( -0.000000000000000000, -0.000000000000000000, -1.000000000000000000 ) ) ;
#6273 = VERTEX_POINT ( 'NONE', #3539 ) ;
#6274 = CARTESIAN_POINT ( 'NONE',  ( 6.495190528383280260, 11.25000000000000000, 0.000000000000000000 ) ) ;
#6275 = CARTESIAN_POINT ( 'NONE',  ( -82.31851962845018988, 52.19907349702081234, 53.24026618324773352 ) ) ;
#6276 = VERTEX_POINT ( 'NONE', #4690 ) ;
#6277 = SURFACE_SIDE_STYLE ('',( #663 ) ) ;
#6278 = DIRECTION ( 'NONE',  ( -0.000000000000000000, 0.000000000000000000, 1.000000000000000000 ) ) ;
#6279 = CARTESIAN_POINT ( 'NONE',  ( 0.000000000000000000, 0.000000000000000000, 82.49999999999998579 ) ) ;
#6280 = EDGE_CURVE ( 'NONE', #6088, #7780, #7171, .T. ) ;
#6281 = CARTESIAN_POINT ( 'NONE',  ( 12.50000000000000000, 25.00000000000000355, 3.703880899869785475E-15 ) ) ;
#6282 = ORIENTED_EDGE ( 'NONE', *, *, #3653, .T. ) ;
#6283 = DIRECTION ( 'NONE',  ( 1.000000000000000000, 0.000000000000000000, 0.000000000000000000 ) ) ;
#6284 = CARTESIAN_POINT ( 'NONE',  ( 373.3169687445243312, 15.68244000841234964, -12.41390036673199759 ) ) ;
#6285 = EDGE_LOOP ( 'NONE', ( #5308, #1935, #5285, #1353 ) ) ;
#6286 = CARTESIAN_POINT ( 'NONE',  ( 162.5000000000000000, 37.50000000000006395, 0.000000000000000000 ) ) ;
#6287 = EDGE_LOOP ( 'NONE', ( #3605, #1572 ) ) ;
#6288 = CARTESIAN_POINT ( 'NONE',  ( 12.50000000000000000, 1.530808498934191127E-15, 2.500000000000085265 ) ) ;
#6289 = DIRECTION ( 'NONE',  ( 1.000000000000000000, 0.000000000000000000, 0.000000000000000000 ) ) ;
#6290 = PRODUCT_DEFINITION_SHAPE ( 'NONE', 'NONE',  #1294 ) ;
#6291 = ORIENTED_EDGE ( 'NONE', *, *, #717, .F. ) ;
#6292 = SHAPE_REPRESENTATION ( 'MAT-014', ( #2064, #406, #1934, #5270, #782, #5399, #6424, #6047, #3747, #149, #1174, #16, #3612, #4494, #2976, #4622, #5911, #659, #2456 ), #4753 ) ;
#6293 = ADVANCED_FACE ( 'NONE', ( #4094 ), #6547, .F. ) ;
#6294 = DIRECTION ( 'NONE',  ( -4.789677997474686366E-16, -1.000000000000000000, -0.000000000000000000 ) ) ;
#6295 = ORIENTED_EDGE ( 'NONE', *, *, #2926, .T. ) ;
#6296 = ORIENTED_EDGE ( 'NONE', *, *, #960, .F. ) ;
#6297 = DIRECTION ( 'NONE',  ( -0.000000000000000000, -0.000000000000000000, -1.000000000000000000 ) ) ;
#6298 = CARTESIAN_POINT ( 'NONE',  ( 50.71904415029504065, 87.70544117646394966, 12.50000000000000000 ) ) ;
#6299 = DIRECTION ( 'NONE',  ( 0.000000000000000000, 0.000000000000000000, -1.000000000000000000 ) ) ;
#6300 = EDGE_LOOP ( 'NONE', ( #640, #1375, #4593, #4033 ) ) ;
#6301 = DIRECTION ( 'NONE',  ( -0.000000000000000000, -0.000000000000000000, 1.000000000000000000 ) ) ;
#6302 = EDGE_CURVE ( 'NONE', #4601, #3485, #4461, .T. ) ;
#6303 = ADVANCED_FACE ( 'NONE', ( #7827, #7791 ), #2336, .F. ) ;
#6304 = ITEM_DEFINED_TRANSFORMATION ( 'NONE', 'NONE', #4494,  #5785 ) ;
#6305 = CARTESIAN_POINT ( 'NONE',  ( 375.0000000000000000, 12.50000000000000000, -12.50000000000000000 ) ) ;
#6306 = DIRECTION ( 'NONE',  ( -1.000000000000000000, 0.000000000000000000, 0.000000000000000000 ) ) ;
#6307 = LINE ( 'NONE', #1534, #3392 ) ;
#6308 = LINE ( 'NONE', #3112, #4794 ) ;
#6309 = EDGE_CURVE ( 'NONE', #7529, #5402, #754, .T. ) ;
#6310 = ORIENTED_EDGE ( 'NONE', *, *, #6839, .F. ) ;
#6311 = DIRECTION ( 'NONE',  ( 0.9335804380297003657, -0.3583679195021128305, 0.000000000000000000 ) ) ;
#6312 = DIRECTION ( 'NONE',  ( 1.000000000000000000, -4.789677997474620299E-16, 1.197598848321618981E-16 ) ) ;
#6314 = ORIENTED_EDGE ( 'NONE', *, *, #1349, .F. ) ;
#6313 = AXIS2_PLACEMENT_3D ( 'NONE', #1481, #4564, #7060 ) ;
#6315 = DIRECTION ( 'NONE',  ( 1.000000000000000000, 0.000000000000000000, 0.000000000000000000 ) ) ;
#6316 = DIRECTION ( 'NONE',  ( 1.000000000000000000, 0.000000000000000000, 0.000000000000000000 ) ) ;
#6317 = DIRECTION ( 'NONE',  ( 1.000000000000000000, -1.295260195396012940E-15, 0.000000000000000000 ) ) ;
#6318 = CARTESIAN_POINT ( 'NONE',  ( 0.000000000000000000, 0.000000000000000000, 25.00000000000000000 ) ) ;
#6319 = ORIENTED_EDGE ( 'NONE', *, *, #2649, .T. ) ;
#6320 = EDGE_CURVE ( 'NONE', #1477, #1859, #4986, .T. ) ;
#6321 = LINE ( 'NONE', #344, #5394 ) ;
#6322 = ORIENTED_EDGE ( 'NONE', *, *, #6249, .F. ) ;
#6323 = LINE ( 'NONE', #229, #4548 ) ;
#6325 = FACE_OUTER_BOUND ( 'NONE', #2000, .T. ) ;
#6324 = VECTOR ( 'NONE', #3025, 1000.000000000000000 ) ;
#6326 = DIRECTION ( 'NONE',  ( 0.000000000000000000, 0.000000000000000000, 1.000000000000000000 ) ) ;
#6327 = DIRECTION ( 'NONE',  ( -0.000000000000000000, 0.000000000000000000, 1.000000000000000000 ) ) ;
#6328 = EDGE_CURVE ( 'NONE', #1785, #6488, #1016, .T. ) ;
#6329 = AXIS2_PLACEMENT_3D ( 'NONE', #7392, #3142, #5049 ) ;
#6330 = ORIENTED_EDGE ( 'NONE', *, *, #1018, .T. ) ;
#6331 = AXIS2_PLACEMENT_3D ( 'NONE', #2099, #5837, #4619 ) ;
#6332 = CARTESIAN_POINT ( 'NONE',  ( 200.0000000000000000, 0.000000000000000000, 12.50000000000000000 ) ) ;
#6333 = ORIENTED_EDGE ( 'NONE', *, *, #6280, .T. ) ;
#6334 = ORIENTED_EDGE ( 'NONE', *, *, #4046, .T. ) ;
#6335 = DIRECTION ( 'NONE',  ( 0.000000000000000000, -1.000000000000000000, 0.000000000000000000 ) ) ;
#6336 = LINE ( 'NONE', #4605, #5937 ) ;
#6337 = CARTESIAN_POINT ( 'NONE',  ( 175.0000000000000000, 0.000000000000000000, 15.00000000000000000 ) ) ;
#6338 = ORIENTED_EDGE ( 'NONE', *, *, #1693, .F. ) ;
#6339 = VECTOR ( 'NONE', #3170, 999.9999999999998863 ) ;
#6340 = CARTESIAN_POINT ( 'NONE',  ( -17.50000000000000355, 0.000000000000000000, 82.49999999999998579 ) ) ;
#6341 = AXIS2_PLACEMENT_3D ( 'NONE', #394, #1153, #7882 ) ;
#6342 = DIRECTION ( 'NONE',  ( 0.000000000000000000, 0.000000000000000000, 1.000000000000000000 ) ) ;
#6343 = LINE ( 'NONE', #5750, #4845 ) ;
#6344 = LINE ( 'NONE', #2051, #6973 ) ;
#6345 = DIRECTION ( 'NONE',  ( 0.000000000000000000, -0.000000000000000000, 1.000000000000000000 ) ) ;
#6346 = EDGE_CURVE ( 'NONE', #4272, #4697, #3454, .T. ) ;
#6347 = AXIS2_PLACEMENT_3D ( 'NONE', #3453, #5976, #1557 ) ;
#6348 = EDGE_CURVE ( 'NONE', #268, #3478, #118, .T. ) ;
#6349 = EDGE_LOOP ( 'NONE', ( #5886, #7027, #1503, #2096, #7675, #7681, #4362 ) ) ;
#6350 = DIRECTION ( 'NONE',  ( 1.000000000000000000, -1.734723475976807094E-15, 0.000000000000000000 ) ) ;
#6351 = AXIS2_PLACEMENT_3D ( 'NONE', #3052, #5568, #2443 ) ;
#6352 = ORIENTED_EDGE ( 'NONE', *, *, #6411, .T. ) ;
#6353 = LINE ( 'NONE', #3309, #2543 ) ;
#6354 = CARTESIAN_POINT ( 'NONE',  ( 5.204170427930428856E-14, 37.50000000000005684, 12.50000000000000000 ) ) ;
#6355 = EDGE_CURVE ( 'NONE', #2065, #30, #6742, .T. ) ;
#6356 = CARTESIAN_POINT ( 'NONE',  ( 412.5000000000000568, 75.00000000000001421, 5.000000000000000000 ) ) ;
#6357 = ORIENTED_EDGE ( 'NONE', *, *, #2342, .T. ) ;
#6358 = PRODUCT_DEFINITION_SHAPE ( 'NONE', 'NONE',  #7917 ) ;
#6359=STYLED_ITEM('',(#7955),#4174);
#6360 = VERTEX_POINT ( 'NONE', #1324 ) ;
#6361 = DIRECTION ( 'NONE',  ( -0.000000000000000000, 0.000000000000000000, 1.000000000000000000 ) ) ;
#6362 = ORIENTED_EDGE ( 'NONE', *, *, #3125, .T. ) ;
#6363 = EDGE_CURVE ( 'NONE', #103, #150, #5230, .T. ) ;
#6364 = DIRECTION ( 'NONE',  ( -1.000000000000000000, 0.000000000000000000, 0.000000000000000000 ) ) ;
#6365 = CIRCLE ( 'NONE', #3166, 12.50000000000001066 ) ;
#6366 = PLANE ( 'NONE',  #1446 ) ;
#6367 = PLANE ( 'NONE',  #6637 ) ;
#6368 = LINE ( 'NONE', #305, #833 ) ;
#6369 = CIRCLE ( 'NONE', #5346, 5.000000000000000888 ) ;
#6370 = ORIENTED_EDGE ( 'NONE', *, *, #2673, .T. ) ;
#6371 = CARTESIAN_POINT ( 'NONE',  ( 0.000000000000000000, 0.000000000000000000, 0.000000000000000000 ) ) ;
#6372 = ORIENTED_EDGE ( 'NONE', *, *, #1309, .F. ) ;
#6373 = VERTEX_POINT ( 'NONE', #4933 ) ;
#6374 = CARTESIAN_POINT ( 'NONE',  ( 212.5000000000000284, 1.530808498934191127E-15, 0.000000000000000000 ) ) ;
#6375 = PLANE ( 'NONE',  #2883 ) ;
#6376 = DIRECTION ( 'NONE',  ( 1.000000000000000000, 0.000000000000000000, 0.000000000000000000 ) ) ;
#6377 = AXIS2_PLACEMENT_3D ( 'NONE', #3851, #796, #723 ) ;
#6378 = LINE ( 'NONE', #6340, #6206 ) ;
#6379 = EDGE_CURVE ( 'NONE', #7849, #7745, #4291, .T. ) ;
#6380 = AXIS2_PLACEMENT_3D ( 'NONE', #6274, #171, #6350 ) ;
#6381 = VECTOR ( 'NONE', #4421, 1000.000000000000000 ) ;
#6382 = ORIENTED_EDGE ( 'NONE', *, *, #6021, .F. ) ;
#6383 = PLANE ( 'NONE',  #4314 ) ;
#6384 = DIRECTION ( 'NONE',  ( 0.7071067811865500152, 0.000000000000000000, -0.7071067811865451302 ) ) ;
#6385 = CARTESIAN_POINT ( 'NONE',  ( 25.71904415029483459, 19.40417101989674009, 12.50000000000000000 ) ) ;
#6386 = FACE_BOUND ( 'NONE', #775, .T. ) ;
#6387 = CIRCLE ( 'NONE', #6526, 29.99999999999997158 ) ;
#6388 =( REPRESENTATION_RELATIONSHIP ('NONE','NONE', #6292, #6910 ) REPRESENTATION_RELATIONSHIP_WITH_TRANSFORMATION ( #252 )SHAPE_REPRESENTATION_RELATIONSHIP( ) );
#6389 = ORIENTED_EDGE ( 'NONE', *, *, #4792, .F. ) ;
#6390 = CARTESIAN_POINT ( 'NONE',  ( -27.49999999999994671, 47.50000000000009237, 0.000000000000000000 ) ) ;
#6391 = AXIS2_PLACEMENT_3D ( 'NONE', #6688, #2969, #6614 ) ;
#6392 = CIRCLE ( 'NONE', #2426, 25.00000000000000711 ) ;
#6393 = DIRECTION ( 'NONE',  ( 0.000000000000000000, 0.000000000000000000, 1.000000000000000000 ) ) ;
#6394 = ORIENTED_EDGE ( 'NONE', *, *, #7091, .F. ) ;
#6395 = SURFACE_STYLE_USAGE ( .BOTH. , #932 ) ;
#6396 = CARTESIAN_POINT ( 'NONE',  ( -37.49999999999989342, 177.4999999999999432, 130.0000000000000000 ) ) ;
#6397 = DIRECTION ( 'NONE',  ( -0.000000000000000000, -0.000000000000000000, -1.000000000000000000 ) ) ;
#6398 = EDGE_CURVE ( 'NONE', #4349, #5068, #3715, .T. ) ;
#6399 = CARTESIAN_POINT ( 'NONE',  ( 0.000000000000000000, 0.000000000000000000, 0.000000000000000000 ) ) ;
#6400 = EDGE_CURVE ( 'NONE', #7887, #2392, #6392, .T. ) ;
#6401 = EDGE_LOOP ( 'NONE', ( #3518, #6759, #6615, #5373 ) ) ;
#6402 = UNCERTAINTY_MEASURE_WITH_UNIT (LENGTH_MEASURE( 1.000000000000000082E-05 ), #2786, 'distance_accuracy_value', 'NONE');
#6403 = ORIENTED_EDGE ( 'NONE', *, *, #3507, .T. ) ;
#6404 = EDGE_CURVE ( 'NONE', #7046, #3816, #1144, .T. ) ;
#6405 = CARTESIAN_POINT ( 'NONE',  ( -61.78095584970497356, 12.70544120911856112, 12.50000000000000000 ) ) ;
#6406 = ORIENTED_EDGE ( 'NONE', *, *, #946, .T. ) ;
#6407 = LINE ( 'NONE', #3442, #602 ) ;
#6408 = ORIENTED_EDGE ( 'NONE', *, *, #1802, .T. ) ;
#6409 = EDGE_CURVE ( 'NONE', #2643, #4500, #5635, .T. ) ;
#6410 = LINE ( 'NONE', #3360, #5172 ) ;
#6411 = EDGE_CURVE ( 'NONE', #1547, #1382, #3180, .T. ) ;
#6412 = ORIENTED_EDGE ( 'NONE', *, *, #1747, .F. ) ;
#6413 = CARTESIAN_POINT ( 'NONE',  ( 52.50000000000000711, 111.9999999999998863, 130.0000000000000000 ) ) ;
#6414 = ORIENTED_EDGE ( 'NONE', *, *, #2959, .T. ) ;
#6415 = DIRECTION ( 'NONE',  ( 0.000000000000000000, 0.000000000000000000, -1.000000000000000000 ) ) ;
#6416 = ORIENTED_EDGE ( 'NONE', *, *, #5917, .T. ) ;
#6417 = DIRECTION ( 'NONE',  ( -0.000000000000000000, -0.000000000000000000, -1.000000000000000000 ) ) ;
#6418 = DIRECTION ( 'NONE',  ( 1.000000000000000000, 0.000000000000000000, 0.000000000000000000 ) ) ;
#6419 = CARTESIAN_POINT ( 'NONE',  ( 42.50000000000000711, 177.5000000000000000, 12.65877081724072362 ) ) ;
#6420 =( GEOMETRIC_REPRESENTATION_CONTEXT ( 3 ) GLOBAL_UNCERTAINTY_ASSIGNED_CONTEXT ( ( #5525 ) ) GLOBAL_UNIT_ASSIGNED_CONTEXT ( ( #5434, #5964, #2839 ) ) REPRESENTATION_CONTEXT ( 'NONE', 'WORKASPACE' ) );
#6421 = ORIENTED_EDGE ( 'NONE', *, *, #1553, .F. ) ;
#6422 = EDGE_CURVE ( 'NONE', #846, #2024, #6823, .T. ) ;
#6423 = PRODUCT_DEFINITION_SHAPE ( 'NONE', 'NONE',  #2231 ) ;
#6424 = AXIS2_PLACEMENT_3D ( 'NONE', #853, #4462, #5103 ) ;
#6425 = FACE_OUTER_BOUND ( 'NONE', #699, .T. ) ;
#6426 = DIRECTION ( 'NONE',  ( -1.000000000000000000, 0.000000000000000000, -0.000000000000000000 ) ) ;
#6427 = FACE_OUTER_BOUND ( 'NONE', #1063, .T. ) ;
#6428 = CARTESIAN_POINT ( 'NONE',  ( 190.0000000000000000, 12.50000000000000000, -15.61249499599599488 ) ) ;
#6429 = LINE ( 'NONE', #6551, #6220 ) ;
#6430 = CARTESIAN_POINT ( 'NONE',  ( 296.6025403784439618, 217.5000000000000568, 125.0000000000000000 ) ) ;
#6431 = VERTEX_POINT ( 'NONE', #612 ) ;
#6432 = CARTESIAN_POINT ( 'NONE',  ( 296.6025403784437913, 82.50000000000004263, 17.49999999999998934 ) ) ;
#6433 = DIRECTION ( 'NONE',  ( -0.000000000000000000, -0.000000000000000000, -1.000000000000000000 ) ) ;
#6434 = APPLICATION_CONTEXT ( 'automotive_design' ) ;
#6435 = ORIENTED_EDGE ( 'NONE', *, *, #5650, .T. ) ;
#6436 = ORIENTED_EDGE ( 'NONE', *, *, #4134, .T. ) ;
#6437 = ORIENTED_EDGE ( 'NONE', *, *, #2526, .F. ) ;
#6438 = CARTESIAN_POINT ( 'NONE',  ( 291.6025403784437913, 135.0000000000000000, 0.000000000000000000 ) ) ;
#6439 = VERTEX_POINT ( 'NONE', #4253 ) ;
#6440 = CARTESIAN_POINT ( 'NONE',  ( 296.6025403784439050, 90.00000000000001421, 12.50000000000000000 ) ) ;
#6441 = ORIENTED_EDGE ( 'NONE', *, *, #4331, .F. ) ;
#6442 = DIRECTION ( 'NONE',  ( -1.000000000000000000, 0.000000000000000000, -0.000000000000000000 ) ) ;
#6443 = DIRECTION ( 'NONE',  ( -0.000000000000000000, -0.000000000000000000, -1.000000000000000000 ) ) ;
#6444 = CIRCLE ( 'NONE', #2997, 5.000000000000004441 ) ;
#6445 = EDGE_CURVE ( 'NONE', #4723, #28, #2163, .T. ) ;
#6446 = ADVANCED_FACE ( 'NONE', ( #3705 ), #5011, .T. ) ;
#6447 = ORIENTED_EDGE ( 'NONE', *, *, #2255, .T. ) ;
#6448 = VECTOR ( 'NONE', #4901, 1000.000000000000000 ) ;
#6449 = CARTESIAN_POINT ( 'NONE',  ( -61.78095584970497356, -62.29455879088143888, 12.50000000000000000 ) ) ;
#6450 = VERTEX_POINT ( 'NONE', #5539 ) ;
#6451 = AXIS2_PLACEMENT_3D ( 'NONE', #5191, #7688, #349 ) ;
#6452 = DIRECTION ( 'NONE',  ( 1.000000000000000000, 0.000000000000000000, 0.000000000000000000 ) ) ;
#6453 = ORIENTED_EDGE ( 'NONE', *, *, #4950, .F. ) ;
#6454 = DIRECTION ( 'NONE',  ( 1.000000000000000000, 0.000000000000000000, -0.000000000000000000 ) ) ;
#6455 = DIRECTION ( 'NONE',  ( 1.000000000000000000, 0.000000000000000000, 0.000000000000000000 ) ) ;
#6456 = CARTESIAN_POINT ( 'NONE',  ( 0.000000000000000000, 0.000000000000000000, 45.00000000000000000 ) ) ;
#6457 = LINE ( 'NONE', #3495, #5948 ) ;
#6458 = AXIS2_PLACEMENT_3D ( 'NONE', #6148, #4447, #5628 ) ;
#6459 = VECTOR ( 'NONE', #2022, 1000.000000000000000 ) ;
#6460 = ORIENTED_EDGE ( 'NONE', *, *, #2070, .F. ) ;
#6461 = CIRCLE ( 'NONE', #3014, 18.00000000000007105 ) ;
#6462 = MECHANICAL_DESIGN_GEOMETRIC_PRESENTATION_REPRESENTATION (  '', ( #4283 ), #453 ) ;
#6463 = FACE_OUTER_BOUND ( 'NONE', #93, .T. ) ;
#6464 = DIRECTION ( 'NONE',  ( -1.000000000000000000, 0.000000000000000000, 0.000000000000000000 ) ) ;
#6465 = DIRECTION ( 'NONE',  ( 0.000000000000000000, 0.000000000000000000, 1.000000000000000000 ) ) ;
#6466 = CARTESIAN_POINT ( 'NONE',  ( -25.00000000000000000, 0.000000000000000000, 0.000000000000000000 ) ) ;
#6467 = DIRECTION ( 'NONE',  ( 1.000000000000000000, 0.000000000000000000, 0.000000000000000000 ) ) ;
#6468 = EDGE_CURVE ( 'NONE', #7527, #150, #683, .T. ) ;
#6469 = VECTOR ( 'NONE', #948, 1000.000000000000000 ) ;
#6470 = CIRCLE ( 'NONE', #2627, 29.99999999999997158 ) ;
#6471 = FACE_OUTER_BOUND ( 'NONE', #401, .T. ) ;
#6472 = DIRECTION ( 'NONE',  ( 1.000000000000000000, -4.789593822244094799E-16, -4.789593822244094799E-16 ) ) ;
#6473 = ORIENTED_EDGE ( 'NONE', *, *, #2919, .T. ) ;
#6474 = DIRECTION ( 'NONE',  ( 0.000000000000000000, -0.000000000000000000, 1.000000000000000000 ) ) ;
#6475 = DIRECTION ( 'NONE',  ( -0.000000000000000000, -0.000000000000000000, -1.000000000000000000 ) ) ;
#6477 = CARTESIAN_POINT ( 'NONE',  ( 412.5000000000000568, 75.00000000000001421, 5.000000000000000000 ) ) ;
#6476 = VECTOR ( 'NONE', #4313, 1000.000000000000000 ) ;
#6478 = FILL_AREA_STYLE ('',( #295 ) ) ;
#6479 = ORIENTED_EDGE ( 'NONE', *, *, #5774, .F. ) ;
#6480 = EDGE_CURVE ( 'NONE', #1507, #4567, #6528, .T. ) ;
#6481 = EDGE_LOOP ( 'NONE', ( #4579, #5776 ) ) ;
#6482 = AXIS2_PLACEMENT_3D ( 'NONE', #7817, #4760, #6415 ) ;
#6483 = VERTEX_POINT ( 'NONE', #3139 ) ;
#6484 = CARTESIAN_POINT ( 'NONE',  ( 162.5000000000000000, 1.990051048614448997E-14, 25.00000000000000000 ) ) ;
#6485 = VERTEX_POINT ( 'NONE', #3853 ) ;
#6486 = DIRECTION ( 'NONE',  ( -0.000000000000000000, -0.000000000000000000, -1.000000000000000000 ) ) ;
#6487 = CARTESIAN_POINT ( 'NONE',  ( 6.249999999999977796, 3.061616997868383043E-15, -25.00000000000000000 ) ) ;
#6488 = VERTEX_POINT ( 'NONE', #2003 ) ;
#6489 = VECTOR ( 'NONE', #3831, 1000.000000000000000 ) ;
#6490 = DIRECTION ( 'NONE',  ( -1.000000000000000000, -0.000000000000000000, -0.000000000000000000 ) ) ;
#6491 = PRODUCT_DEFINITION_SHAPE ( 'NONE', 'NONE',  #1538 ) ;
#6492 = EDGE_LOOP ( 'NONE', ( #789, #5395, #6813, #5283 ) ) ;
#6493 = AXIS2_PLACEMENT_3D ( 'NONE', #4411, #2010, #1929 ) ;
#6494 = CARTESIAN_POINT ( 'NONE',  ( 412.4999999999998863, 82.50000000000004263, 17.49999999999998934 ) ) ;
#6495 = ORIENTED_EDGE ( 'NONE', *, *, #6816, .T. ) ;
#6496 = DIRECTION ( 'NONE',  ( 1.000000000000000000, -9.251858538542979716E-16, 0.000000000000000000 ) ) ;
#6497 = ORIENTED_EDGE ( 'NONE', *, *, #76, .T. ) ;
#6498 =( REPRESENTATION_RELATIONSHIP ('NONE','NONE', #6292, #341 ) REPRESENTATION_RELATIONSHIP_WITH_TRANSFORMATION ( #6304 )SHAPE_REPRESENTATION_RELATIONSHIP( ) );
#6499 = DIRECTION ( 'NONE',  ( -1.000000000000000000, 0.000000000000000000, -0.000000000000000000 ) ) ;
#6500 = DIRECTION ( 'NONE',  ( 1.000000000000000000, 0.000000000000000000, -0.000000000000000000 ) ) ;
#6501 = CARTESIAN_POINT ( 'NONE',  ( -16.96112411586215529, 80.38061160285559481, 12.50000000000000000 ) ) ;
#6502 = EDGE_CURVE ( 'NONE', #3550, #2505, #4444, .T. ) ;
#6503 = CARTESIAN_POINT ( 'NONE',  ( 0.000000000000000000, 0.000000000000000000, 97.50000000000000000 ) ) ;
#6504 = CONICAL_SURFACE ( 'NONE', #5986, 12.50000000000000000, 0.7853981633974491672 ) ;
#6505 = EDGE_CURVE ( 'NONE', #4567, #1507, #249, .T. ) ;
#6506 = ORIENTED_EDGE ( 'NONE', *, *, #2979, .F. ) ;
#6507 = EDGE_CURVE ( 'NONE', #6766, #6240, #7580, .T. ) ;
#6508 = VECTOR ( 'NONE', #4364, 1000.000000000000000 ) ;
#6509 = CARTESIAN_POINT ( 'NONE',  ( 0.000000000000000000, 0.000000000000000000, 2.000000000000001776 ) ) ;
#6510 = CARTESIAN_POINT ( 'NONE',  ( 0.000000000000000000, 0.000000000000000000, 92.50000000000000000 ) ) ;
#6511 = DIRECTION ( 'NONE',  ( 1.000000000000000000, 1.040834085586084257E-15, 0.000000000000000000 ) ) ;
#6512 = FACE_OUTER_BOUND ( 'NONE', #6928, .T. ) ;
#6513 = CARTESIAN_POINT ( 'NONE',  ( -25.00000000000000000, 25.00000000000000000, 0.000000000000000000 ) ) ;
#6514 = AXIS2_PLACEMENT_3D ( 'NONE', #3930, #6376, #5087 ) ;
#6515 = VECTOR ( 'NONE', #5106, 1000.000000000000000 ) ;
#6516 = ADVANCED_FACE ( 'NONE', ( #7464 ), #1526, .F. ) ;
#6517 = DIRECTION ( 'NONE',  ( 0.5000000000000000000, 0.8660254037844385966, 0.000000000000000000 ) ) ;
#6518 = CARTESIAN_POINT ( 'NONE',  ( 257.3507467850105286, 209.6990734970208905, 252.0932327501082568 ) ) ;
#6519 = VERTEX_POINT ( 'NONE', #283 ) ;
#6520 = AXIS2_PLACEMENT_3D ( 'NONE', #7728, #4077, #4672 ) ;
#6521 = DIRECTION ( 'NONE',  ( -0.000000000000000000, -0.000000000000000000, -1.000000000000000000 ) ) ;
#6522 = CIRCLE ( 'NONE', #366, 12.50000000000000000 ) ;
#6523 = DIRECTION ( 'NONE',  ( -1.000000000000000000, 0.000000000000000000, 0.000000000000000000 ) ) ;
#6524 =( NAMED_UNIT ( * ) SI_UNIT ( $, .STERADIAN. ) SOLID_ANGLE_UNIT ( ) );
#6525 = ORIENTED_EDGE ( 'NONE', *, *, #1400, .T. ) ;
#6526 = AXIS2_PLACEMENT_3D ( 'NONE', #4859, #7316, #4257 ) ;
#6527 = ORIENTED_EDGE ( 'NONE', *, *, #760, .T. ) ;
#6528 = CIRCLE ( 'NONE', #7295, 12.50000000000000355 ) ;
#6529 = ORIENTED_EDGE ( 'NONE', *, *, #7065, .F. ) ;
#6530 = ORIENTED_EDGE ( 'NONE', *, *, #3168, .T. ) ;
#6531 = EDGE_CURVE ( 'NONE', #3303, #603, #3335, .T. ) ;
#6532 = FACE_OUTER_BOUND ( 'NONE', #3238, .T. ) ;
#6533 = DIRECTION ( 'NONE',  ( -0.000000000000000000, -0.000000000000000000, -1.000000000000000000 ) ) ;
#6534 = VERTEX_POINT ( 'NONE', #5700 ) ;
#6535 = DIRECTION ( 'NONE',  ( 0.000000000000000000, -1.000000000000000000, 0.000000000000000000 ) ) ;
#6536 = CARTESIAN_POINT ( 'NONE',  ( 0.000000000000000000, 0.000000000000000000, 82.49999999999998579 ) ) ;
#6537 = ORIENTED_EDGE ( 'NONE', *, *, #1940, .F. ) ;
#6538 = DIRECTION ( 'NONE',  ( -0.000000000000000000, -0.000000000000000000, -1.000000000000000000 ) ) ;
#6539 = ORIENTED_EDGE ( 'NONE', *, *, #5819, .T. ) ;
#6540 = DIRECTION ( 'NONE',  ( 1.000000000000000000, 0.000000000000000000, 0.000000000000000000 ) ) ;
#6541 = ORIENTED_EDGE ( 'NONE', *, *, #5473, .F. ) ;
#6542 = CARTESIAN_POINT ( 'NONE',  ( 400.0000000000000000, 0.000000000000000000, 0.000000000000000000 ) ) ;
#6543 = DIRECTION ( 'NONE',  ( 0.000000000000000000, 0.000000000000000000, 1.000000000000000000 ) ) ;
#6544 = ORIENTED_EDGE ( 'NONE', *, *, #1165, .T. ) ;
#6545 = VERTEX_POINT ( 'NONE', #2729 ) ;
#6546 = FACE_BOUND ( 'NONE', #6287, .T. ) ;
#6547 = CYLINDRICAL_SURFACE ( 'NONE', #5630, 12.50000000000000000 ) ;
#6548 = DIRECTION ( 'NONE',  ( 1.000000000000000000, 4.789677997474691297E-16, -0.000000000000000000 ) ) ;
#6549 = AXIS2_PLACEMENT_3D ( 'NONE', #6438, #2796, #4626 ) ;
#6550 = CARTESIAN_POINT ( 'NONE',  ( 0.000000000000000000, 0.000000000000000000, 77.49999999999998579 ) ) ;
#6551 = CARTESIAN_POINT ( 'NONE',  ( 9.381941874331417353, -16.24999999999999645, 7.500000000000000000 ) ) ;
#6552 = ADVANCED_FACE ( 'NONE', ( #6978 ), #1957, .T. ) ;
#6553 = EDGE_CURVE ( 'NONE', #7894, #7492, #6865, .T. ) ;
#6554 = PRODUCT_DEFINITION_FORMATION_WITH_SPECIFIED_SOURCE ( 'ANY', '', #3221, .NOT_KNOWN. ) ;
#6555 = CARTESIAN_POINT ( 'NONE',  ( 0.000000000000000000, 1.836970198721029589E-15, -15.00000000000000000 ) ) ;
#6556 = DIRECTION ( 'NONE',  ( 0.000000000000000000, 0.000000000000000000, 1.000000000000000000 ) ) ;
#6557 = EDGE_LOOP ( 'NONE', ( #4542, #4248, #7713, #2787, #4166 ) ) ;
#6558 = DIRECTION ( 'NONE',  ( -0.000000000000000000, 0.000000000000000000, 1.000000000000000000 ) ) ;
#6559 = CARTESIAN_POINT ( 'NONE',  ( -25.00000000000000000, 24.99999999999999289, 50.00000000000000000 ) ) ;
#6560 = PLANE ( 'NONE',  #1087 ) ;
#6561 = VERTEX_POINT ( 'NONE', #2651 ) ;
#6562 = EDGE_CURVE ( 'NONE', #3264, #136, #3372, .T. ) ;
#6563 = ORIENTED_EDGE ( 'NONE', *, *, #7864, .T. ) ;
#6564 = ORIENTED_EDGE ( 'NONE', *, *, #1448, .T. ) ;
#6565 = PRESENTATION_STYLE_ASSIGNMENT (( #4112 ) ) ;
#6566 = DIRECTION ( 'NONE',  ( 0.000000000000000000, 0.000000000000000000, 1.000000000000000000 ) ) ;
#6567 = ORIENTED_EDGE ( 'NONE', *, *, #5020, .T. ) ;
#6568 = PLANE ( 'NONE',  #3314 ) ;
#6569 = DIRECTION ( 'NONE',  ( 0.000000000000000000, 0.000000000000000000, 1.000000000000000000 ) ) ;
#6570 = EDGE_CURVE ( 'NONE', #107, #3922, #1763, .T. ) ;
#6571 = ORIENTED_EDGE ( 'NONE', *, *, #4090, .T. ) ;
#6572 = LINE ( 'NONE', #4120, #2816 ) ;
#6573 = ORIENTED_EDGE ( 'NONE', *, *, #525, .T. ) ;
#6574 = DIRECTION ( 'NONE',  ( 1.000000000000000000, 0.000000000000000000, 0.000000000000000000 ) ) ;
#6575 = ORIENTED_EDGE ( 'NONE', *, *, #7296, .F. ) ;
#6576 = DIRECTION ( 'NONE',  ( 1.000000000000000000, 0.000000000000000000, 0.000000000000000000 ) ) ;
#6577 = PLANE ( 'NONE',  #7872 ) ;
#6578 = VERTEX_POINT ( 'NONE', #842 ) ;
#6579 = CLOSED_SHELL ( 'NONE', ( #4685, #1622, #3211, #3029, #1734, #5429, #7346, #633, #6303, #6869, #7341 ) ) ;
#6580 = ORIENTED_EDGE ( 'NONE', *, *, #5293, .T. ) ;
#6581 = CYLINDRICAL_SURFACE ( 'NONE', #7270, 24.99999996734539209 ) ;
#6582 = DIRECTION ( 'NONE',  ( 0.8886649088774989380, -0.4585571717133497538, 0.000000000000000000 ) ) ;
#6583 = CARTESIAN_POINT ( 'NONE',  ( 47.50000000000000711, 177.5000000000000000, 5.000000000000000000 ) ) ;
#6584 = VECTOR ( 'NONE', #6067, 1000.000000000000000 ) ;
#6585 = VECTOR ( 'NONE', #3682, 999.9999999999998863 ) ;
#6586 = LINE ( 'NONE', #7793, #6584 ) ;
#6587 = LINE ( 'NONE', #1092, #6984 ) ;
#6588 = VECTOR ( 'NONE', #6189, 1000.000000000000000 ) ;
#6589 = CIRCLE ( 'NONE', #5440, 37.50000000000000711 ) ;
#6590 = FACE_OUTER_BOUND ( 'NONE', #2845, .T. ) ;
#6591 = CARTESIAN_POINT ( 'NONE',  ( 124.0868394622074504, 184.1990734970206063, 183.2402661832477406 ) ) ;
#6592 = VERTEX_POINT ( 'NONE', #883 ) ;
#6593 = EDGE_CURVE ( 'NONE', #2348, #4343, #234, .T. ) ;
#6594 = DIRECTION ( 'NONE',  ( -0.7071067811865502373, 8.659560562354966138E-17, 0.7071067811865447972 ) ) ;
#6595 = CARTESIAN_POINT ( 'NONE',  ( 286.6025403784439050, 0.000000000000000000, 12.50000000000000000 ) ) ;
#6596 = DIRECTION ( 'NONE',  ( 0.000000000000000000, -1.000000000000000000, 0.000000000000000000 ) ) ;
#6597 = ORIENTED_EDGE ( 'NONE', *, *, #2533, .F. ) ;
#6598 = CIRCLE ( 'NONE', #2369, 20.00000000000000000 ) ;
#6599 = ADVANCED_FACE ( 'NONE', ( #4724 ), #5615, .T. ) ;
#6600 = CIRCLE ( 'NONE', #191, 25.00000000000000000 ) ;
#6601 = CIRCLE ( 'NONE', #2449, 12.49999999999999467 ) ;
#6602 = ORIENTED_EDGE ( 'NONE', *, *, #5885, .T. ) ;
#6603 = VECTOR ( 'NONE', #3343, 1000.000000000000114 ) ;
#6604 = EDGE_CURVE ( 'NONE', #7913, #1554, #2208, .T. ) ;
#6605 = EDGE_LOOP ( 'NONE', ( #1878, #300 ) ) ;
#6606 = EDGE_CURVE ( 'NONE', #6264, #334, #404, .T. ) ;
#6607 = CARTESIAN_POINT ( 'NONE',  ( 46.25000000000002842, 111.9999999999999005, 130.0000000000000000 ) ) ;
#6608 = CARTESIAN_POINT ( 'NONE',  ( 190.0000000000000000, 0.000000000000000000, 0.000000000000000000 ) ) ;
#6609 = VERTEX_POINT ( 'NONE', #2167 ) ;
#6610 = CARTESIAN_POINT ( 'NONE',  ( 162.5000000000000000, 112.5000000000000142, 0.000000000000000000 ) ) ;
#6611 = CIRCLE ( 'NONE', #4167, 12.49999999999999822 ) ;
#6612 = ORIENTED_EDGE ( 'NONE', *, *, #3611, .F. ) ;
#6613 = ADVANCED_FACE ( 'NONE', ( #7099 ), #5332, .F. ) ;
#6614 = DIRECTION ( 'NONE',  ( 1.000000000000000000, 0.000000000000000000, 0.000000000000000000 ) ) ;
#6615 = ORIENTED_EDGE ( 'NONE', *, *, #7864, .F. ) ;
#6616 = CARTESIAN_POINT ( 'NONE',  ( 362.8413258170837707, -19.78835583758980832, 2.930536303278098664 ) ) ;
#6617 = VERTEX_POINT ( 'NONE', #7819 ) ;
#6618 = CARTESIAN_POINT ( 'NONE',  ( 37.50000000000000711, 42.50000000000003553, 12.50000000000000000 ) ) ;
#6619 = DIRECTION ( 'NONE',  ( 0.000000000000000000, -1.000000000000000000, 0.000000000000000000 ) ) ;
#6620 = CIRCLE ( 'NONE', #1875, 5.000000000000000000 ) ;
#6621 = ORIENTED_EDGE ( 'NONE', *, *, #6169, .F. ) ;
#6622 = ORIENTED_EDGE ( 'NONE', *, *, #2721, .F. ) ;
#6623 = EDGE_CURVE ( 'NONE', #6254, #7564, #5868, .T. ) ;
#6624 = DIRECTION ( 'NONE',  ( -0.000000000000000000, 0.000000000000000000, -1.000000000000000000 ) ) ;
#6625 = DIRECTION ( 'NONE',  ( 0.000000000000000000, -1.000000000000000000, 0.000000000000000000 ) ) ;
#6627 = DIRECTION ( 'NONE',  ( 0.000000000000000000, 0.000000000000000000, 1.000000000000000000 ) ) ;
#6626 = AXIS2_PLACEMENT_3D ( 'NONE', #1688, #1203, #7151 ) ;
#6628 = CARTESIAN_POINT ( 'NONE',  ( 212.5000000000000284, 1.530808498934191127E-15, 12.50000000000000000 ) ) ;
#6629 = CARTESIAN_POINT ( 'NONE',  ( 380.6272118725746623, 16.58005916595991280, -11.19168395254304471 ) ) ;
#6630 = AXIS2_PLACEMENT_3D ( 'NONE', #1361, #2648, #7019 ) ;
#6631 = DIRECTION ( 'NONE',  ( 0.000000000000000000, 1.000000000000000000, -0.000000000000000000 ) ) ;
#6632 = APPLICATION_PROTOCOL_DEFINITION ( 'draft international standard', 'automotive_design', 1998, #3731 ) ;
#6633 = CARTESIAN_POINT ( 'NONE',  ( 150.0000000000000000, 1.836970198721029747E-14, 25.00000000000000000 ) ) ;
#6634 = DIRECTION ( 'NONE',  ( 1.000000000000000000, 0.000000000000000000, 0.000000000000000000 ) ) ;
#6635 = CARTESIAN_POINT ( 'NONE',  ( -27.49999999999994671, 47.50000000000009237, 12.65877081724073783 ) ) ;
#6636 = CARTESIAN_POINT ( 'NONE',  ( 17.50000000000000355, 2.143131898507868643E-15, 77.49999999999998579 ) ) ;
#6638 = VERTEX_POINT ( 'NONE', #4048 ) ;
#6637 = AXIS2_PLACEMENT_3D ( 'NONE', #232, #3805, #2681 ) ;
#6639 = AXIS2_PLACEMENT_3D ( 'NONE', #1978, #6837, #2468 ) ;
#6640 = EDGE_CURVE ( 'NONE', #5516, #7370, #6128, .T. ) ;
#6641 = VERTEX_POINT ( 'NONE', #6501 ) ;
#6642 = VERTEX_POINT ( 'NONE', #5203 ) ;
#6643 = ORIENTED_EDGE ( 'NONE', *, *, #3424, .F. ) ;
#6644 = DIRECTION ( 'NONE',  ( 0.000000000000000000, 0.000000000000000000, 1.000000000000000000 ) ) ;
#6645 = LINE ( 'NONE', #7130, #686 ) ;
#6646 = ORIENTED_EDGE ( 'NONE', *, *, #4852, .T. ) ;
#6647 = CARTESIAN_POINT ( 'NONE',  ( 0.000000000000000000, -25.00000000000000000, 0.000000000000000000 ) ) ;
#6648 = VECTOR ( 'NONE', #4519, 1000.000000000000000 ) ;
#6649 = AXIS2_PLACEMENT_3D ( 'NONE', #2415, #6701, #1204 ) ;
#6650 = APPLICATION_CONTEXT ( 'automotive_design' ) ;
#6651 = EDGE_CURVE ( 'NONE', #5267, #4433, #3184, .T. ) ;
#6652 = ORIENTED_EDGE ( 'NONE', *, *, #1420, .F. ) ;
#6653 = EDGE_CURVE ( 'NONE', #4276, #1620, #2328, .T. ) ;
#6654 = CYLINDRICAL_SURFACE ( 'NONE', #4983, 12.50000000000001066 ) ;
#6655 = ORIENTED_EDGE ( 'NONE', *, *, #7339, .F. ) ;
#6656 = CIRCLE ( 'NONE', #1909, 12.50000000000001066 ) ;
#6657 = CARTESIAN_POINT ( 'NONE',  ( 363.8177372226678017, -19.20332549959546853, -5.601192942097885208 ) ) ;
#6658 = VECTOR ( 'NONE', #3648, 1000.000000000000000 ) ;
#6659 = ORIENTED_EDGE ( 'NONE', *, *, #2673, .F. ) ;
#6660 = LINE ( 'NONE', #7892, #2253 ) ;
#6661 = EDGE_CURVE ( 'NONE', #2900, #5478, #4836, .T. ) ;
#6662 = ORIENTED_EDGE ( 'NONE', *, *, #4235, .T. ) ;
#6663 = ORIENTED_EDGE ( 'NONE', *, *, #6023, .T. ) ;
#6664 = DIRECTION ( 'NONE',  ( -0.000000000000000000, -0.000000000000000000, -1.000000000000000000 ) ) ;
#6665 = LINE ( 'NONE', #7789, #86 ) ;
#6666 = DIRECTION ( 'NONE',  ( 1.000000000000000000, 0.000000000000000000, 0.000000000000000000 ) ) ;
#6667 = CARTESIAN_POINT ( 'NONE',  ( 353.4483633286965301, 217.5000000000000284, 138.3903618369216417 ) ) ;
#6668 = DIRECTION ( 'NONE',  ( -1.000000000000000000, -0.000000000000000000, -0.000000000000000000 ) ) ;
#6669 = CARTESIAN_POINT ( 'NONE',  ( 46.25000000000002842, 47.50000000000003553, 130.0000000000000000 ) ) ;
#6670 = EDGE_CURVE ( 'NONE', #109, #4276, #4071, .T. ) ;
#6671 = CARTESIAN_POINT ( 'NONE',  ( 0.000000000000000000, 0.000000000000000000, 52.50000000000000000 ) ) ;
#6672 = PRODUCT_CONTEXT ( 'NONE', #2184, 'mechanical' ) ;
#6673 = FACE_OUTER_BOUND ( 'NONE', #6019, .T. ) ;
#6674 = CARTESIAN_POINT ( 'NONE',  ( -27.08354679051378255, 47.50000000000009948, 12.55124306091977182 ) ) ;
#6675 = PLANE ( 'NONE',  #3003 ) ;
#6676 = CIRCLE ( 'NONE', #4871, 24.99999996734560881 ) ;
#6677 = ORIENTED_EDGE ( 'NONE', *, *, #2987, .F. ) ;
#6678 = ORIENTED_EDGE ( 'NONE', *, *, #2340, .F. ) ;
#6679 = DIRECTION ( 'NONE',  ( 0.000000000000000000, 0.000000000000000000, 1.000000000000000000 ) ) ;
#6680 = FACE_OUTER_BOUND ( 'NONE', #3243, .T. ) ;
#6681 = CARTESIAN_POINT ( 'NONE',  ( -27.49999999999989342, 182.4999999999999432, 12.50000000000000000 ) ) ;
#6682 = CYLINDRICAL_SURFACE ( 'NONE', #3645, 25.00000000000000000 ) ;
#6683 = CARTESIAN_POINT ( 'NONE',  ( 0.000000000000000000, 0.000000000000000000, 77.49999999999998579 ) ) ;
#6684 = VERTEX_POINT ( 'NONE', #7740 ) ;
#6685 = DIRECTION ( 'NONE',  ( 1.000000000000000000, 0.000000000000000000, 0.000000000000000000 ) ) ;
#6686 = EDGE_CURVE ( 'NONE', #6044, #7015, #445, .T. ) ;
#6687 = EDGE_LOOP ( 'NONE', ( #7490, #2713, #5981, #1084, #5291, #3943, #550, #6119 ) ) ;
#6688 = CARTESIAN_POINT ( 'NONE',  ( -49.28095584970496645, -62.29455879088143888, 12.50000000000000000 ) ) ;
#6689 = ORIENTED_EDGE ( 'NONE', *, *, #5725, .F. ) ;
#6690 = CARTESIAN_POINT ( 'NONE',  ( 366.7466773492281504, -17.65289753843946841, 9.421765557058566998 ) ) ;
#6691 = EDGE_LOOP ( 'NONE', ( #1791, #7048, #4318, #6770 ) ) ;
#6692 = EDGE_CURVE ( 'NONE', #3005, #7842, #7656, .T. ) ;
#6693 = DIRECTION ( 'NONE',  ( 0.000000000000000000, -0.000000000000000000, -1.000000000000000000 ) ) ;
#6694 = CYLINDRICAL_SURFACE ( 'NONE', #963, 5.000000000000000888 ) ;
#6695 = EDGE_CURVE ( 'NONE', #5006, #6642, #4606, .T. ) ;
#6696 = ORIENTED_EDGE ( 'NONE', *, *, #6309, .F. ) ;
#6697 = ORIENTED_EDGE ( 'NONE', *, *, #2265, .F. ) ;
#6698 = ADVANCED_FACE ( 'NONE', ( #3571 ), #6020, .T. ) ;
#6699 = PLANE ( 'NONE',  #4831 ) ;
#6700 = DIRECTION ( 'NONE',  ( 0.000000000000000000, 0.000000000000000000, -1.000000000000000000 ) ) ;
#6701 = DIRECTION ( 'NONE',  ( -1.000000000000000000, -0.000000000000000000, -0.000000000000000000 ) ) ;
#6702 = CARTESIAN_POINT ( 'NONE',  ( 162.5000000000000000, 112.5000000000000142, 12.50000000000000000 ) ) ;
#6703 = CARTESIAN_POINT ( 'NONE',  ( -4.731064025391297956E-15, 37.50000000000004263, 0.000000000000000000 ) ) ;
#6704 = CARTESIAN_POINT ( 'NONE',  ( 0.7190441502950353225, 62.70544120911855401, 12.50000000000000000 ) ) ;
#6705 = CARTESIAN_POINT ( 'NONE',  ( 52.50000000000000711, 111.9999999999999858, 130.0000000000000000 ) ) ;
#6706 = VECTOR ( 'NONE', #3067, 1000.000000000000000 ) ;
#6707 = APPLICATION_PROTOCOL_DEFINITION ( 'draft international standard', 'automotive_design', 1998, #4943 ) ;
#6708 = CLOSED_SHELL ( 'NONE', ( #6138, #5079, #4725, #3849, #687, #1441, #2243, #4185, #2389, #4243, #1492, #5983, #2474, #2749, #135, #5323, #1564, #5740, #303, #4342, #1933 ) ) ;
#6709 = CARTESIAN_POINT ( 'NONE',  ( 0.000000000000000000, 0.000000000000000000, 2.000000000000001776 ) ) ;
#6710 = CARTESIAN_POINT ( 'NONE',  ( 0.000000000000000000, 0.000000000000000000, 0.000000000000000000 ) ) ;
#6711 = EDGE_CURVE ( 'NONE', #869, #334, #6894, .T. ) ;
#6712 = DIRECTION ( 'NONE',  ( -0.000000000000000000, -0.000000000000000000, -1.000000000000000000 ) ) ;
#6713 = VECTOR ( 'NONE', #3107, 1000.000000000000000 ) ;
#6714 = ORIENTED_EDGE ( 'NONE', *, *, #7535, .F. ) ;
#6715 = ORIENTED_EDGE ( 'NONE', *, *, #2157, .T. ) ;
#6716 = DIRECTION ( 'NONE',  ( 1.000000000000000000, 0.000000000000000000, 0.000000000000000000 ) ) ;
#6717 = CARTESIAN_POINT ( 'NONE',  ( 375.0000000000000000, -12.50000000000000355, 12.50000000000000711 ) ) ;
#6719 = PLANE ( 'NONE',  #575 ) ;
#6718 = AXIS2_PLACEMENT_3D ( 'NONE', #7023, #1603, #4049 ) ;
#6720 = VECTOR ( 'NONE', #3158, 1000.000000000000000 ) ;
#6721 = CIRCLE ( 'NONE', #3893, 12.50000000000000000 ) ;
#6722 = EDGE_CURVE ( 'NONE', #5081, #2041, #3307, .T. ) ;
#6723 = DIRECTION ( 'NONE',  ( -0.000000000000000000, -0.000000000000000000, -1.000000000000000000 ) ) ;
#6724 = EDGE_LOOP ( 'NONE', ( #3394, #1517 ) ) ;
#6725 = DIRECTION ( 'NONE',  ( 0.000000000000000000, 1.000000000000000000, 0.000000000000000000 ) ) ;
#6726 = ORIENTED_EDGE ( 'NONE', *, *, #7308, .T. ) ;
#6727 = CARTESIAN_POINT ( 'NONE',  ( 362.6036394379159447, 19.93536271250352598, 1.660494579713906127 ) ) ;
#6728 = VERTEX_POINT ( 'NONE', #5249 ) ;
#6729 = CARTESIAN_POINT ( 'NONE',  ( 363.6408507984733660, -19.30709367143974831, -5.233317247790644444 ) ) ;
#6730 = ORIENTED_EDGE ( 'NONE', *, *, #4738, .F. ) ;
#6731 = FACE_OUTER_BOUND ( 'NONE', #3762, .T. ) ;
#6732 = AXIS2_PLACEMENT_3D ( 'NONE', #3763, #3640, #6242 ) ;
#6733 = DIRECTION ( 'NONE',  ( -0.000000000000000000, -0.000000000000000000, -1.000000000000000000 ) ) ;
#6734 = ORIENTED_EDGE ( 'NONE', *, *, #5163, .F. ) ;
#6735 = ADVANCED_FACE ( 'NONE', ( #7700 ), #4642, .F. ) ;
#6736 = CIRCLE ( 'NONE', #2899, 18.75000000000009948 ) ;
#6737 = ORIENTED_EDGE ( 'NONE', *, *, #2046, .T. ) ;
#6738 = VERTEX_POINT ( 'NONE', #4921 ) ;
#6739 = EDGE_CURVE ( 'NONE', #5478, #7566, #2974, .T. ) ;
#6740 = CARTESIAN_POINT ( 'NONE',  ( 362.5000000000001137, -4.592425496802567267E-15, 0.000000000000000000 ) ) ;
#6741 = CARTESIAN_POINT ( 'NONE',  ( 387.0561628848909663, -19.72539574521466932, -3.327763323014857555 ) ) ;
#6742 = LINE ( 'NONE', #4214, #1910 ) ;
#6743 = CARTESIAN_POINT ( 'NONE',  ( 12.50000000000000000, 1.530808498934191521E-15, 0.000000000000000000 ) ) ;
#6744 = LINE ( 'NONE', #4407, #2237 ) ;
#6745 = CIRCLE ( 'NONE', #976, 11.64999999999996660 ) ;
#6746 = EDGE_CURVE ( 'NONE', #1386, #6179, #7532, .T. ) ;
#6747 = EDGE_CURVE ( 'NONE', #2269, #6578, #1759, .T. ) ;
#6748 = CARTESIAN_POINT ( 'NONE',  ( 291.6025403784439050, 90.00000000000001421, 12.50000000000000000 ) ) ;
#6749 = AXIS2_PLACEMENT_3D ( 'NONE', #5720, #3757, #4464 ) ;
#6750 = EDGE_CURVE ( 'NONE', #7220, #7046, #4880, .T. ) ;
#6751 = CONTEXT_DEPENDENT_SHAPE_REPRESENTATION ( #3114, #912 ) ;
#6752 = CYLINDRICAL_SURFACE ( 'NONE', #1242, 12.50000000000001066 ) ;
#6753 = CARTESIAN_POINT ( 'NONE',  ( 190.0000000000000000, -12.50000000000000000, -21.65063509461096913 ) ) ;
#6754 = DIRECTION ( 'NONE',  ( 1.000000000000000000, 0.000000000000000000, 0.000000000000000000 ) ) ;
#6755 = CARTESIAN_POINT ( 'NONE',  ( 199.9999999999998863, 225.0000000000000284, 12.50000000000000000 ) ) ;
#6756 = EDGE_CURVE ( 'NONE', #6264, #7209, #3131, .T. ) ;
#6757 = EDGE_CURVE ( 'NONE', #1141, #6738, #2199, .T. ) ;
#6758 = AXIS2_PLACEMENT_3D ( 'NONE', #969, #5252, #1532 ) ;
#6759 = ORIENTED_EDGE ( 'NONE', *, *, #420, .F. ) ;
#6760 = ORIENTED_EDGE ( 'NONE', *, *, #7483, .T. ) ;
#6761 = CARTESIAN_POINT ( 'NONE',  ( 125.0000000000000000, 0.000000000000000000, 0.000000000000000000 ) ) ;
#6762 = CARTESIAN_POINT ( 'NONE',  ( 0.7190441502950353225, 62.70544120911855401, 12.50000000000000000 ) ) ;
#6763 = AXIS2_PLACEMENT_3D ( 'NONE', #4484, #7616, #7577 ) ;
#6764 = CARTESIAN_POINT ( 'NONE',  ( -17.32050807568877104, 2.500000000000002220, 7.500000000000000000 ) ) ;
#6765 = PRESENTATION_STYLE_ASSIGNMENT (( #4833 ) ) ;
#6766 = VERTEX_POINT ( 'NONE', #5407 ) ;
#6767 = CARTESIAN_POINT ( 'NONE',  ( 47.36967921662626679, 6.904171036223937463, 12.50000000000000000 ) ) ;
#6768=STYLED_ITEM('',(#7962),#6795);
#6769 = AXIS2_PLACEMENT_3D ( 'NONE', #4045, #3967, #3456 ) ;
#6770 = ORIENTED_EDGE ( 'NONE', *, *, #2314, .T. ) ;
#6771 = EDGE_CURVE ( 'NONE', #7160, #2126, #6252, .T. ) ;
#6772 = CARTESIAN_POINT ( 'NONE',  ( -61.78095584970497356, -62.29455879088143888, 12.50000000000000000 ) ) ;
#6773 = VERTEX_POINT ( 'NONE', #6814 ) ;
#6774 = CARTESIAN_POINT ( 'NONE',  ( 362.5234216988060894, -19.98534102192048323, 0.8725863811532602599 ) ) ;
#6775 = ORIENTED_EDGE ( 'NONE', *, *, #4894, .F. ) ;
#6776 = CARTESIAN_POINT ( 'NONE',  ( 232.4759526419164786, -18.74999999999998934, 12.50000000000000000 ) ) ;
#6777 = CIRCLE ( 'NONE', #4589, 35.78244274809159720 ) ;
#6778 = PLANE ( 'NONE',  #1599 ) ;
#6779 = ORIENTED_EDGE ( 'NONE', *, *, #5326, .F. ) ;
#6780 = CIRCLE ( 'NONE', #1656, 12.50000000000001066 ) ;
#6781 = VECTOR ( 'NONE', #2820, 1000.000000000000227 ) ;
#6782 = ORIENTED_EDGE ( 'NONE', *, *, #5133, .T. ) ;
#6783 = EDGE_LOOP ( 'NONE', ( #5363, #6001, #2202, #6233 ) ) ;
#6784 = DIRECTION ( 'NONE',  ( -1.000000000000000000, 0.000000000000000000, 0.000000000000000000 ) ) ;
#6785 = DIRECTION ( 'NONE',  ( -0.000000000000000000, -0.000000000000000000, -1.000000000000000000 ) ) ;
#6786 = CARTESIAN_POINT ( 'NONE',  ( 375.0000000000000000, 12.50000000000000000, 3.061616997868383043E-15 ) ) ;
#6787 = LINE ( 'NONE', #7390, #7089 ) ;
#6788 = CARTESIAN_POINT ( 'NONE',  ( -37.49999999999989342, 177.4999999999999432, 12.50000000000000000 ) ) ;
#6789 = PRODUCT_CONTEXT ( 'NONE', #6182, 'mechanical' ) ;
#6790 = CARTESIAN_POINT ( 'NONE',  ( 162.4999999999999432, 187.4999999999999716, 12.50000000000000000 ) ) ;
#6791 = CARTESIAN_POINT ( 'NONE',  ( 63.21904415029505486, 62.70544120911855401, 12.50000000000000000 ) ) ;
#6792 = CYLINDRICAL_SURFACE ( 'NONE', #2246, 12.50000000000000000 ) ;
#6793 = CARTESIAN_POINT ( 'NONE',  ( 0.000000000000000000, 0.000000000000000000, 90.00000000000000000 ) ) ;
#6794 = ADVANCED_FACE ( 'NONE', ( #7852, #6731, #3609, #1195, #3695, #675 ), #1916, .F. ) ;
#6795 = MANIFOLD_SOLID_BREP ( 'Pah2', #566 ) ;
#6796 = EDGE_CURVE ( 'NONE', #2057, #7215, #31, .T. ) ;
#6797 = ORIENTED_EDGE ( 'NONE', *, *, #6746, .F. ) ;
#6798 = APPLICATION_CONTEXT ( 'automotive_design' ) ;
#6799 =( NAMED_UNIT ( * ) PLANE_ANGLE_UNIT ( ) SI_UNIT ( $, .RADIAN. ) );
#6800 = VERTEX_POINT ( 'NONE', #7891 ) ;
#6801 = DIRECTION ( 'NONE',  ( 0.000000000000000000, 0.000000000000000000, 1.000000000000000000 ) ) ;
#6802 = DIRECTION ( 'NONE',  ( -0.000000000000000000, -0.000000000000000000, -1.000000000000000000 ) ) ;
#6803 = FACE_OUTER_BOUND ( 'NONE', #6285, .T. ) ;
#6804 = LINE ( 'NONE', #1381, #6720 ) ;
#6805 = VERTEX_POINT ( 'NONE', #4203 ) ;
#6806 = LINE ( 'NONE', #3160, #6603 ) ;
#6807 = UNCERTAINTY_MEASURE_WITH_UNIT (LENGTH_MEASURE( 1.000000000000000082E-05 ), #4486, 'distance_accuracy_value', 'NONE');
#6808 = ORIENTED_EDGE ( 'NONE', *, *, #2485, .F. ) ;
#6809 = PLANE ( 'NONE',  #1783 ) ;
#6810 = PLANE ( 'NONE',  #5742 ) ;
#6811 = EDGE_LOOP ( 'NONE', ( #5617, #4182, #737, #3600 ) ) ;
#6812 = CARTESIAN_POINT ( 'NONE',  ( 49.37500000000001421, 112.5000000000000142, 195.4980915752512658 ) ) ;
#6813 = ORIENTED_EDGE ( 'NONE', *, *, #1728, .F. ) ;
#6814 = CARTESIAN_POINT ( 'NONE',  ( -27.49999999999994671, 37.50000000000008527, 12.50000000000000000 ) ) ;
#6815 = DIRECTION ( 'NONE',  ( -0.000000000000000000, -0.000000000000000000, 1.000000000000000000 ) ) ;
#6816 = EDGE_CURVE ( 'NONE', #308, #784, #1378, .T. ) ;
#6817 = VERTEX_POINT ( 'NONE', #5493 ) ;
#6818 = ORIENTED_EDGE ( 'NONE', *, *, #7432, .T. ) ;
#6819 = EDGE_LOOP ( 'NONE', ( #7697, #6597, #3800, #2768 ) ) ;
#6820 = CARTESIAN_POINT ( 'NONE',  ( 13.21904415029503355, 62.70544120911855401, 0.000000000000000000 ) ) ;
#6821 = AXIS2_PLACEMENT_3D ( 'NONE', #4692, #7153, #2494 ) ;
#6822 = CARTESIAN_POINT ( 'NONE',  ( 386.6750961250273235, -19.49464854461726304, 4.484522112394339288 ) ) ;
#6823 = LINE ( 'NONE', #2569, #2170 ) ;
#6824 = DIRECTION ( 'NONE',  ( -0.000000000000000000, -0.000000000000000000, -1.000000000000000000 ) ) ;
#6825 = DIRECTION ( 'NONE',  ( -1.000000000000000000, 0.000000000000000000, 0.000000000000000000 ) ) ;
#6826 = CONTEXT_DEPENDENT_SHAPE_REPRESENTATION ( #5775, #6358 ) ;
#6827 = DIRECTION ( 'NONE',  ( -0.000000000000000000, 0.000000000000000000, 1.000000000000000000 ) ) ;
#6828 = CARTESIAN_POINT ( 'NONE',  ( -12.50000000000000000, 0.000000000000000000, 0.5000000000000004441 ) ) ;
#6829 = CARTESIAN_POINT ( 'NONE',  ( 0.000000000000000000, 0.000000000000000000, 90.00000000000000000 ) ) ;
#6830 = FACE_OUTER_BOUND ( 'NONE', #5933, .T. ) ;
#6831 = ORIENTED_EDGE ( 'NONE', *, *, #4331, .T. ) ;
#6832 = VECTOR ( 'NONE', #5248, 1000.000000000000000 ) ;
#6833 = ADVANCED_FACE ( 'NONE', ( #2481 ), #1392, .F. ) ;
#6834 =( NAMED_UNIT ( * ) SI_UNIT ( $, .STERADIAN. ) SOLID_ANGLE_UNIT ( ) );
#6835 = ORIENTED_EDGE ( 'NONE', *, *, #2573, .T. ) ;
#6836 = DIRECTION ( 'NONE',  ( -1.000000000000000000, 0.000000000000000000, 0.000000000000000000 ) ) ;
#6837 = DIRECTION ( 'NONE',  ( 0.000000000000000000, 0.000000000000000000, 1.000000000000000000 ) ) ;
#6838 = CARTESIAN_POINT ( 'NONE',  ( 17.50000000000000355, 2.143131898507868643E-15, 92.50000000000000000 ) ) ;
#6839 = EDGE_CURVE ( 'NONE', #600, #2766, #4393, .T. ) ;
#6840 = CARTESIAN_POINT ( 'NONE',  ( -25.00000000000000000, 0.000000000000000000, 0.000000000000000000 ) ) ;
#6841 = ORIENTED_EDGE ( 'NONE', *, *, #6858, .T. ) ;
#6842 = CIRCLE ( 'NONE', #4269, 5.000000000000004441 ) ;
#6843 = CARTESIAN_POINT ( 'NONE',  ( 0.000000000000000000, 0.000000000000000000, 45.00000000000000000 ) ) ;
#6844 = AXIS2_PLACEMENT_3D ( 'NONE', #6124, #141, #1939 ) ;
#6845 = ADVANCED_FACE ( 'NONE', ( #5004, #3281 ), #6367, .F. ) ;
#6846 = APPLICATION_CONTEXT ( 'automotive_design' ) ;
#6847 = ORIENTED_EDGE ( 'NONE', *, *, #5885, .F. ) ;
#6848 = EDGE_CURVE ( 'NONE', #3797, #5144, #2719, .T. ) ;
#6849 = CARTESIAN_POINT ( 'NONE',  ( 363.3249038749727333, 19.49464854461726304, 4.484522112394339288 ) ) ;
#6850 = AXIS2_PLACEMENT_3D ( 'NONE', #3119, #634, #403 ) ;
#6851 = ORIENTED_EDGE ( 'NONE', *, *, #3656, .T. ) ;
#6852 = CARTESIAN_POINT ( 'NONE',  ( 12.50000000000000000, 1.530808498934191127E-15, 45.00000000000000000 ) ) ;
#6853 = ORIENTED_EDGE ( 'NONE', *, *, #5561, .T. ) ;
#6854 = FACE_OUTER_BOUND ( 'NONE', #843, .T. ) ;
#6855 = DIRECTION ( 'NONE',  ( -1.000000000000000000, 4.270088556250607616E-16, -0.000000000000000000 ) ) ;
#6856 = AXIS2_PLACEMENT_3D ( 'NONE', #489, #4846, #1164 ) ;
#6857 = AXIS2_PLACEMENT_3D ( 'NONE', #132, #1447, #49 ) ;
#6858 = EDGE_CURVE ( 'NONE', #4661, #6638, #5148, .T. ) ;
#6859 = ORIENTED_EDGE ( 'NONE', *, *, #1587, .T. ) ;
#6860 = ORIENTED_EDGE ( 'NONE', *, *, #3496, .F. ) ;
#6861 = AXIS2_PLACEMENT_3D ( 'NONE', #1707, #7256, #4154 ) ;
#6862 = ORIENTED_EDGE ( 'NONE', *, *, #76, .F. ) ;
#6863 = LINE ( 'NONE', #3813, #3181 ) ;
#6864 = CARTESIAN_POINT ( 'NONE',  ( 378.3038998296499926, -15.95358756117676258, -12.06260739558933714 ) ) ;
#6865 = LINE ( 'NONE', #1363, #3700 ) ;
#6866 = ORIENTED_EDGE ( 'NONE', *, *, #2349, .F. ) ;
#6867 = CARTESIAN_POINT ( 'NONE',  ( -61.78095584970497356, 12.70544120911856112, 12.50000000000000000 ) ) ;
#6868 = AXIS2_PLACEMENT_3D ( 'NONE', #5145, #5805, #1582 ) ;
#6869 = ADVANCED_FACE ( 'NONE', ( #3169 ), #5098, .T. ) ;
#6870 = PRODUCT_DEFINITION_SHAPE ( 'NONE', 'NONE',  #4475 ) ;
#6871 = DIRECTION ( 'NONE',  ( -1.000000000000000000, 0.000000000000000000, 0.000000000000000000 ) ) ;
#6872 = CARTESIAN_POINT ( 'NONE',  ( 387.5000000000000568, 0.000000000000000000, 0.000000000000000000 ) ) ;
#6874 = CARTESIAN_POINT ( 'NONE',  ( 42.50000000000000711, 177.5000000000000000, 12.50000000000000000 ) ) ;
#6873 = COLOUR_RGB ( '',0.7921568627450980005, 0.8196078431372548767, 0.9333333333333333481 ) ;
#6875 = CARTESIAN_POINT ( 'NONE',  ( 46.25000000000002842, 47.50000000000003553, 17.50000000000001421 ) ) ;
#6876 = ORIENTED_EDGE ( 'NONE', *, *, #3488, .T. ) ;
#6877 = COLOUR_RGB ( '',0.7921568627450980005, 0.8196078431372548767, 0.9333333333333333481 ) ;
#6878 = LINE ( 'NONE', #3904, #5357 ) ;
#6879 = EDGE_LOOP ( 'NONE', ( #2075, #7611, #7055, #2604 ) ) ;
#6880 = CARTESIAN_POINT ( 'NONE',  ( -36.78095584970496645, -62.29455879088143888, 0.000000000000000000 ) ) ;
#6881 = DIRECTION ( 'NONE',  ( 0.000000000000000000, 1.000000000000000000, 0.000000000000000000 ) ) ;
#6882 = LINE ( 'NONE', #1307, #3263 ) ;
#6883 = ORIENTED_EDGE ( 'NONE', *, *, #414, .F. ) ;
#6884 = CARTESIAN_POINT ( 'NONE',  ( 381.6490413535094035, 16.96668907523693548, 10.59241602951089867 ) ) ;
#6885 = PRODUCT_DEFINITION ( 'UNKNOWN', '', #3106, #3985 ) ;
#6886 = UNCERTAINTY_MEASURE_WITH_UNIT (LENGTH_MEASURE( 1.000000000000000082E-05 ), #1146, 'distance_accuracy_value', 'NONE');
#6887 = AXIS2_PLACEMENT_3D ( 'NONE', #5581, #7345, #3657 ) ;
#6888 = CARTESIAN_POINT ( 'NONE',  ( 363.8044315608395323, 19.21001202690979781, 5.620007094727602848 ) ) ;
#6889 = VERTEX_POINT ( 'NONE', #4555 ) ;
#6890 = LINE ( 'NONE', #5002, #1737 ) ;
#6891 = VERTEX_POINT ( 'NONE', #271 ) ;
#6892 = CARTESIAN_POINT ( 'NONE',  ( 190.0000000000000000, -12.50000000000000000, -15.61249499599599488 ) ) ;
#6893 = DIRECTION ( 'NONE',  ( -0.000000000000000000, -0.000000000000000000, -1.000000000000000000 ) ) ;
#6894 = CIRCLE ( 'NONE', #4575, 25.00000003264134918 ) ;
#6895 = ADVANCED_FACE ( 'NONE', ( #6854 ), #7607, .F. ) ;
#6896 = AXIS2_PLACEMENT_3D ( 'NONE', #2550, #4379, #741 ) ;
#6897 = ADVANCED_FACE ( 'NONE', ( #2640 ), #7011, .T. ) ;
#6898 = VERTEX_POINT ( 'NONE', #753 ) ;
#6899 = DIRECTION ( 'NONE',  ( 1.000000000000000000, 0.000000000000000000, 0.000000000000000000 ) ) ;
#6900 = VERTEX_POINT ( 'NONE', #1949 ) ;
#6901 = PRESENTATION_LAYER_ASSIGNMENT (  '', '', ( #4714 ) ) ;
#6902 = CIRCLE ( 'NONE', #878, 12.50000000000000000 ) ;
#6903 = ORIENTED_EDGE ( 'NONE', *, *, #364, .T. ) ;
#6904 = CARTESIAN_POINT ( 'NONE',  ( 11.46392929283375928, -22.21662272193747256, 0.000000000000000000 ) ) ;
#6905 = CARTESIAN_POINT ( 'NONE',  ( 387.1601938586447318, -19.78928940797825931, -2.924464941254242056 ) ) ;
#6906 = DIRECTION ( 'NONE',  ( 0.000000000000000000, 1.000000000000000000, 0.000000000000000000 ) ) ;
#6907 = ORIENTED_EDGE ( 'NONE', *, *, #1027, .T. ) ;
#6908 = ADVANCED_FACE ( 'NONE', ( #3208, #1354 ), #5653, .F. ) ;
#6909 = CARTESIAN_POINT ( 'NONE',  ( 9.381941874331406694, 16.25000000000000000, 7.500000000000000000 ) ) ;
#6910 = SHAPE_REPRESENTATION ( 'Bolt3', ( #5785 ), #2702 ) ;
#6911 = VECTOR ( 'NONE', #6105, 1000.000000000000000 ) ;
#6912 = FACE_OUTER_BOUND ( 'NONE', #5184, .T. ) ;
#6913 = DIRECTION ( 'NONE',  ( 0.000000000000000000, -1.387778780781445676E-16, 1.000000000000000000 ) ) ;
#6914 = CARTESIAN_POINT ( 'NONE',  ( 286.6025403784439050, 75.00000000000002842, 0.000000000000000000 ) ) ;
#6915 = DIRECTION ( 'NONE',  ( 0.000000000000000000, 0.000000000000000000, 1.000000000000000000 ) ) ;
#6916 = EDGE_CURVE ( 'NONE', #4834, #1320, #4434, .T. ) ;
#6917 = ORIENTED_EDGE ( 'NONE', *, *, #3057, .T. ) ;
#6918 = DIRECTION ( 'NONE',  ( -0.000000000000000000, 0.000000000000000000, 1.000000000000000000 ) ) ;
#6919 = DIRECTION ( 'NONE',  ( -4.789678059278511676E-16, -1.000000000000000000, -1.093553141097136260E-21 ) ) ;
#6920 = ORIENTED_EDGE ( 'NONE', *, *, #5117, .T. ) ;
#6921 = FACE_OUTER_BOUND ( 'NONE', #996, .T. ) ;
#6922 = DIRECTION ( 'NONE',  ( 1.000000000000000000, 0.000000000000000000, 0.000000000000000000 ) ) ;
#6923 = DIRECTION ( 'NONE',  ( -0.000000000000000000, -0.000000000000000000, -1.000000000000000000 ) ) ;
#6924 = CYLINDRICAL_SURFACE ( 'NONE', #5166, 25.00000003264134918 ) ;
#6925 = ORIENTED_EDGE ( 'NONE', *, *, #2206, .T. ) ;
#6926 = VERTEX_POINT ( 'NONE', #6288 ) ;
#6927 = DIRECTION ( 'NONE',  ( 0.000000000000000000, 0.000000000000000000, 1.000000000000000000 ) ) ;
#6928 = EDGE_LOOP ( 'NONE', ( #5336, #2475, #1159, #5028 ) ) ;
#6929 = DIRECTION ( 'NONE',  ( 0.000000000000000000, 0.000000000000000000, 1.000000000000000000 ) ) ;
#6930 = EDGE_LOOP ( 'NONE', ( #74, #3080 ) ) ;
#6931 = PLANE ( 'NONE',  #627 ) ;
#6932 = DIRECTION ( 'NONE',  ( -0.000000000000000000, -0.000000000000000000, -1.000000000000000000 ) ) ;
#6933 = PRODUCT ( 'Joint Plane', 'Joint Plane', '', ( #7276 ) ) ;
#6934 = PRODUCT_DEFINITION_FORMATION_WITH_SPECIFIED_SOURCE ( 'ANY', '', #3858, .NOT_KNOWN. ) ;
#6935 = EDGE_LOOP ( 'NONE', ( #2404, #4363, #874, #2437 ) ) ;
#6936 = LINE ( 'NONE', #995, #6648 ) ;
#6937 = ORIENTED_EDGE ( 'NONE', *, *, #2484, .T. ) ;
#6938 = EDGE_CURVE ( 'NONE', #2333, #6684, #872, .T. ) ;
#6939 = ORIENTED_EDGE ( 'NONE', *, *, #1528, .T. ) ;
#6940 = DIRECTION ( 'NONE',  ( -1.000000000000000000, -1.295260195396013137E-15, 0.000000000000000000 ) ) ;
#6941 = CARTESIAN_POINT ( 'NONE',  ( 326.6025403784437913, 142.5000000000000000, 125.0000000000000000 ) ) ;
#6942 = CARTESIAN_POINT ( 'NONE',  ( 412.5000000000002274, 1.221245327087672598E-12, 12.50000000000000000 ) ) ;
#6943 = ORIENTED_EDGE ( 'NONE', *, *, #2635, .F. ) ;
#6944 = EDGE_CURVE ( 'NONE', #7782, #7250, #2542, .T. ) ;
#6945 = DIRECTION ( 'NONE',  ( -0.000000000000000000, -0.000000000000000000, -1.000000000000000000 ) ) ;
#6946 = ADVANCED_FACE ( 'NONE', ( #2033, #4476 ), #6931, .F. ) ;
#6947 = DIRECTION ( 'NONE',  ( 1.000000000000000000, 0.000000000000000000, 0.000000000000000000 ) ) ;
#6948 = CARTESIAN_POINT ( 'NONE',  ( 25.71904415029483459, -5.595828947448873159, 0.000000000000000000 ) ) ;
#6949 = CYLINDRICAL_SURFACE ( 'NONE', #4533, 65.50000000000000000 ) ;
#6950 = LINE ( 'NONE', #2052, #6070 ) ;
#6951 =( REPRESENTATION_RELATIONSHIP ('NONE','NONE', #6292, #341 ) REPRESENTATION_RELATIONSHIP_WITH_TRANSFORMATION ( #688 )SHAPE_REPRESENTATION_RELATIONSHIP( ) );
#6952 = ORIENTED_EDGE ( 'NONE', *, *, #3855, .F. ) ;
#6953 = DIRECTION ( 'NONE',  ( -0.3583679195021128305, -0.9335804380297003657, 0.000000000000000000 ) ) ;
#6954 = DIRECTION ( 'NONE',  ( -0.1693361248670392505, 8.110460059738896747E-17, 0.9855583578941505829 ) ) ;
#6955 = ORIENTED_EDGE ( 'NONE', *, *, #473, .T. ) ;
#6956 =( LENGTH_UNIT ( ) NAMED_UNIT ( * ) SI_UNIT ( .MILLI., .METRE. ) );
#6957 = CARTESIAN_POINT ( 'NONE',  ( 325.0000000000000000, 12.50000000000000000, 25.00000000000000000 ) ) ;
#6958 = LINE ( 'NONE', #3310, #3134 ) ;
#6959 = DIRECTION ( 'NONE',  ( -1.000000000000000000, 0.000000000000000000, 0.000000000000000000 ) ) ;
#6960 = ORIENTED_EDGE ( 'NONE', *, *, #2888, .F. ) ;
#6961 = UNCERTAINTY_MEASURE_WITH_UNIT (LENGTH_MEASURE( 1.000000000000000082E-05 ), #4632, 'distance_accuracy_value', 'NONE');
#6962 = DIRECTION ( 'NONE',  ( -0.7071067811865517916, 8.659560562354985860E-17, 0.7071067811865431318 ) ) ;
#6963 = ORIENTED_EDGE ( 'NONE', *, *, #1080, .T. ) ;
#6964 = ADVANCED_FACE ( 'NONE', ( #831, #2071 ), #6969, .F. ) ;
#6965 = LINE ( 'NONE', #6812, #7626 ) ;
#6967 = DIRECTION ( 'NONE',  ( -0.000000000000000000, -0.000000000000000000, -1.000000000000000000 ) ) ;
#6966 = VECTOR ( 'NONE', #3377, 1000.000000000000000 ) ;
#6968 = VECTOR ( 'NONE', #703, 1000.000000000000000 ) ;
#6969 = PLANE ( 'NONE',  #3823 ) ;
#6970 = DIRECTION ( 'NONE',  ( -0.000000000000000000, -0.000000000000000000, -1.000000000000000000 ) ) ;
#6971 = VECTOR ( 'NONE', #7409, 1000.000000000000000 ) ;
#6972 = ORIENTED_EDGE ( 'NONE', *, *, #787, .F. ) ;
#6973 = VECTOR ( 'NONE', #7624, 1000.000000000000000 ) ;
#6974 = FACE_OUTER_BOUND ( 'NONE', #1899, .T. ) ;
#6975 = ORIENTED_EDGE ( 'NONE', *, *, #1111, .F. ) ;
#6976 = ORIENTED_EDGE ( 'NONE', *, *, #5419, .T. ) ;
#6977 = DIRECTION ( 'NONE',  ( 1.000000000000000000, 0.000000000000000000, -0.000000000000000000 ) ) ;
#6978 = FACE_OUTER_BOUND ( 'NONE', #6219, .T. ) ;
#6979 = AXIS2_PLACEMENT_3D ( 'NONE', #1760, #1718, #6543 ) ;
#6980 = VECTOR ( 'NONE', #3871, 1000.000000000000000 ) ;
#6981 = CIRCLE ( 'NONE', #3525, 25.00000000000000711 ) ;
#6982 = FACE_OUTER_BOUND ( 'NONE', #4323, .T. ) ;
#6983 = PRODUCT_RELATED_PRODUCT_CATEGORY ( 'part', '', ( #2848 ) ) ;
#6984 = VECTOR ( 'NONE', #2986, 1000.000000000000000 ) ;
#6985 = ADVANCED_FACE ( 'NONE', ( #5279 ), #2284, .F. ) ;
#6986 = EDGE_LOOP ( 'NONE', ( #7557, #450, #7636, #3384 ) ) ;
#6987 = CARTESIAN_POINT ( 'NONE',  ( 400.0000000000000568, 0.000000000000000000, 25.00000000000000000 ) ) ;
#6988 = CARTESIAN_POINT ( 'NONE',  ( 400.0000000000000568, 0.000000000000000000, 0.000000000000000000 ) ) ;
#6989 = DIRECTION ( 'NONE',  ( -0.000000000000000000, 0.000000000000000000, -1.000000000000000000 ) ) ;
#6990 = FACE_OUTER_BOUND ( 'NONE', #2559, .T. ) ;
#6991 = VECTOR ( 'NONE', #186, 1000.000000000000000 ) ;
#6992 = ADVANCED_FACE ( 'NONE', ( #5891 ), #6568, .F. ) ;
#6993 = EDGE_LOOP ( 'NONE', ( #3756, #773 ) ) ;
#6994 = ADVANCED_FACE ( 'NONE', ( #350 ), #3993, .F. ) ;
#6995 = DIRECTION ( 'NONE',  ( 0.000000000000000000, -0.000000000000000000, 1.000000000000000000 ) ) ;
#6996 = ORIENTED_EDGE ( 'NONE', *, *, #5584, .T. ) ;
#6997 = DIRECTION ( 'NONE',  ( 1.000000000000000000, 0.000000000000000000, 0.000000000000000000 ) ) ;
#6998 = DIRECTION ( 'NONE',  ( -0.000000000000000000, -0.000000000000000000, -1.000000000000000000 ) ) ;
#6999 = FACE_OUTER_BOUND ( 'NONE', #193, .T. ) ;
#7000 = FACE_OUTER_BOUND ( 'NONE', #4702, .T. ) ;
#7001 = ORIENTED_EDGE ( 'NONE', *, *, #4107, .T. ) ;
#7002 = ADVANCED_FACE ( 'NONE', ( #4037, #5238 ), #2801, .F. ) ;
#7003 = PRODUCT_DEFINITION_SHAPE ( 'NONE', 'NONE',  #7920 ) ;
#7004 = AXIS2_PLACEMENT_3D ( 'NONE', #3793, #6198, #6315 ) ;
#7005 = LINE ( 'NONE', #3874, #3837 ) ;
#7006 = ORIENTED_EDGE ( 'NONE', *, *, #3675, .T. ) ;
#7007 = CARTESIAN_POINT ( 'NONE',  ( -25.00000000000000000, 0.000000000000000000, -25.00000000000000000 ) ) ;
#7008 = VECTOR ( 'NONE', #2656, 1000.000000000000000 ) ;
#7009 = CARTESIAN_POINT ( 'NONE',  ( -26.66645320948611442, 177.5512430609197168, 12.50000000000001421 ) ) ;
#7010 = MANIFOLD_SOLID_BREP ( 'Pah1', #2090 ) ;
#7011 = PLANE ( 'NONE',  #3447 ) ;
#7012 = PLANE ( 'NONE',  #4155 ) ;
#7013 = ADVANCED_FACE ( 'NONE', ( #2846 ), #947, .T. ) ;
#7014 = AXIS2_PLACEMENT_3D ( 'NONE', #5739, #3775, #5123 ) ;
#7015 = VERTEX_POINT ( 'NONE', #7132 ) ;
#7016 = CARTESIAN_POINT ( 'NONE',  ( 158.9591979875528409, 23.33951095074252891, 25.00000000000000000 ) ) ;
#7017 = ORIENTED_EDGE ( 'NONE', *, *, #2070, .T. ) ;
#7018 = ORIENTED_EDGE ( 'NONE', *, *, #7145, .F. ) ;
#7019 = DIRECTION ( 'NONE',  ( 1.000000000000000000, 0.000000000000000000, 0.000000000000000000 ) ) ;
#7020 = VECTOR ( 'NONE', #5453, 1000.000000000000000 ) ;
#7021 = CARTESIAN_POINT ( 'NONE',  ( 286.6025403784437913, 150.0000000000000284, 0.000000000000000000 ) ) ;
#7022 = AXIS2_PLACEMENT_3D ( 'NONE', #1480, #5780, #1435 ) ;
#7023 = CARTESIAN_POINT ( 'NONE',  ( -49.28095584970496645, 12.70544120911856112, 12.50000000000000000 ) ) ;
#7024 = MANIFOLD_SOLID_BREP ( 'Pah1', #4271 ) ;
#7025 = AXIS2_PLACEMENT_3D ( 'NONE', #7772, #6442, #7645 ) ;
#7026 = VECTOR ( 'NONE', #2706, 1000.000000000000000 ) ;
#7027 = ORIENTED_EDGE ( 'NONE', *, *, #1061, .T. ) ;
#7028 = CARTESIAN_POINT ( 'NONE',  ( -31.24999999999997158, 113.0000000000000995, 130.0000000000000000 ) ) ;
#7029 = DIRECTION ( 'NONE',  ( -0.000000000000000000, -0.000000000000000000, -1.000000000000000000 ) ) ;
#7030 = FACE_OUTER_BOUND ( 'NONE', #1022, .T. ) ;
#7031 = CARTESIAN_POINT ( 'NONE',  ( 362.5000000000001137, -4.592425496802567267E-15, 25.00000000000000000 ) ) ;
#7032 = CIRCLE ( 'NONE', #2809, 32.75000000000000000 ) ;
#7033 = CIRCLE ( 'NONE', #2804, 12.50000000000001066 ) ;
#7034 = CYLINDRICAL_SURFACE ( 'NONE', #5963, 12.50000000000001066 ) ;
#7035 = CARTESIAN_POINT ( 'NONE',  ( 125.0000000000000000, 0.000000000000000000, 0.000000000000000000 ) ) ;
#7036 = AXIS2_PLACEMENT_3D ( 'NONE', #6245, #710, #2594 ) ;
#7037 = AXIS2_PLACEMENT_3D ( 'NONE', #1089, #3419, #5864 ) ;
#7038 = ORIENTED_EDGE ( 'NONE', *, *, #2187, .F. ) ;
#7039 = ADVANCED_FACE ( 'NONE', ( #7590, #7476 ), #1034, .F. ) ;
#7040 = DIRECTION ( 'NONE',  ( 0.000000000000000000, -0.000000000000000000, -1.000000000000000000 ) ) ;
#7041 = FACE_OUTER_BOUND ( 'NONE', #2620, .T. ) ;
#7042 = FACE_OUTER_BOUND ( 'NONE', #2589, .T. ) ;
#7043 = FACE_BOUND ( 'NONE', #3278, .T. ) ;
#7044 = ORIENTED_EDGE ( 'NONE', *, *, #5412, .T. ) ;
#7045 = EDGE_CURVE ( 'NONE', #5686, #5728, #2026, .T. ) ;
#7046 = VERTEX_POINT ( 'NONE', #6390 ) ;
#7047 = DIRECTION ( 'NONE',  ( -0.000000000000000000, 0.000000000000000000, 1.000000000000000000 ) ) ;
#7048 = ORIENTED_EDGE ( 'NONE', *, *, #4428, .F. ) ;
#7049 = CYLINDRICAL_SURFACE ( 'NONE', #2514, 12.50000000000000355 ) ;
#7050 = FACE_OUTER_BOUND ( 'NONE', #5076, .T. ) ;
#7051 = DIRECTION ( 'NONE',  ( -1.000000000000000000, 0.000000000000000000, 0.000000000000000000 ) ) ;
#7052 = CARTESIAN_POINT ( 'NONE',  ( -74.28095588234631919, 12.70544120911856112, 0.000000000000000000 ) ) ;
#7053 = ORIENTED_EDGE ( 'NONE', *, *, #5412, .F. ) ;
#7054 = DIRECTION ( 'NONE',  ( 1.000000000000000000, 0.000000000000000000, 0.000000000000000000 ) ) ;
#7055 = ORIENTED_EDGE ( 'NONE', *, *, #6258, .T. ) ;
#7056 = CYLINDRICAL_SURFACE ( 'NONE', #3033, 25.00000000000000000 ) ;
#7057 = ORIENTED_EDGE ( 'NONE', *, *, #1177, .F. ) ;
#7058 = CARTESIAN_POINT ( 'NONE',  ( 42.50000000000000711, 187.5000000000000000, 12.50000000000000000 ) ) ;
#7059 = EDGE_CURVE ( 'NONE', #7780, #530, #2055, .T. ) ;
#7060 = DIRECTION ( 'NONE',  ( 1.000000000000000000, 0.000000000000000000, 0.000000000000000000 ) ) ;
#7061 = DIRECTION ( 'NONE',  ( -1.000000000000000000, 0.000000000000000000, 0.000000000000000000 ) ) ;
#7062 = DIRECTION ( 'NONE',  ( -1.000000000000000000, -0.000000000000000000, -0.000000000000000000 ) ) ;
#7063 = AXIS2_PLACEMENT_3D ( 'NONE', #5844, #1546, #299 ) ;
#7064 = ORIENTED_EDGE ( 'NONE', *, *, #7308, .F. ) ;
#7065 = EDGE_CURVE ( 'NONE', #4126, #6519, #183, .T. ) ;
#7066 = EDGE_CURVE ( 'NONE', #7370, #4834, #5388, .T. ) ;
#7067 = CARTESIAN_POINT ( 'NONE',  ( -12.50000000000000000, -25.00000000000000355, 37.50000000000000000 ) ) ;
#7068 = CYLINDRICAL_SURFACE ( 'NONE', #242, 4.999999999999997335 ) ;
#7069 = CARTESIAN_POINT ( 'NONE',  ( -27.49999999999989342, 177.4999999999999432, 0.000000000000000000 ) ) ;
#7070 = CARTESIAN_POINT ( 'NONE',  ( 62.50000000000009948, 144.7499999999999147, 130.0000000000000000 ) ) ;
#7071 = CARTESIAN_POINT ( 'NONE',  ( 384.8819872053468885, 18.47584224143657039, 7.665216593424116986 ) ) ;
#7072 = CARTESIAN_POINT ( 'NONE',  ( 13.00000000000000178, 0.000000000000000000, 6.999999999999999112 ) ) ;
#7073 = DIRECTION ( 'NONE',  ( 1.000000000000000000, -4.789593822244094799E-16, -4.789593822244094799E-16 ) ) ;
#7074 = ORIENTED_EDGE ( 'NONE', *, *, #3090, .F. ) ;
#7075 = CARTESIAN_POINT ( 'NONE',  ( -25.00000000000000000, 25.00000000000000000, 0.000000000000000000 ) ) ;
#7076 = LINE ( 'NONE', #294, #7744 ) ;
#7077 = FACE_BOUND ( 'NONE', #3941, .T. ) ;
#7078 = EDGE_LOOP ( 'NONE', ( #6621, #7662 ) ) ;
#7079 = EDGE_CURVE ( 'NONE', #6641, #784, #5639, .T. ) ;
#7080 = ORIENTED_EDGE ( 'NONE', *, *, #6379, .T. ) ;
#7081 = VERTEX_POINT ( 'NONE', #893 ) ;
#7082 = ADVANCED_FACE ( 'NONE', ( #5715 ), #3228, .F. ) ;
#7083 = CARTESIAN_POINT ( 'NONE',  ( 75.00000000000000000, 10.56842436860067735, 25.00000000000000000 ) ) ;
#7084 = ORIENTED_EDGE ( 'NONE', *, *, #900, .F. ) ;
#7085 = CYLINDRICAL_SURFACE ( 'NONE', #6868, 5.000000000000000888 ) ;
#7086 = ORIENTED_EDGE ( 'NONE', *, *, #4218, .F. ) ;
#7087 = ORIENTED_EDGE ( 'NONE', *, *, #5133, .F. ) ;
#7088 = CARTESIAN_POINT ( 'NONE',  ( 37.50000000000000711, 42.50000000000003553, 12.50000000000000000 ) ) ;
#7089 = VECTOR ( 'NONE', #7271, 1000.000000000000000 ) ;
#7090 = EDGE_CURVE ( 'NONE', #7849, #6534, #7798, .T. ) ;
#7091 = EDGE_CURVE ( 'NONE', #5144, #5833, #4843, .T. ) ;
#7092 = ORIENTED_EDGE ( 'NONE', *, *, #7148, .T. ) ;
#7093 = CIRCLE ( 'NONE', #318, 37.50000000000000000 ) ;
#7094 = CARTESIAN_POINT ( 'NONE',  ( 296.6025403784437913, 144.9999999999999716, 5.000000000000000000 ) ) ;
#7095 = ORIENTED_EDGE ( 'NONE', *, *, #1052, .F. ) ;
#7096 = CARTESIAN_POINT ( 'NONE',  ( -26.24999999999997158, 177.6587708172406224, 12.50000000000000000 ) ) ;
#7097 = VERTEX_POINT ( 'NONE', #5674 ) ;
#7098 = DIRECTION ( 'NONE',  ( -1.000000000000000000, 0.000000000000000000, 0.000000000000000000 ) ) ;
#7099 = FACE_OUTER_BOUND ( 'NONE', #5880, .T. ) ;
#7100 = FACE_OUTER_BOUND ( 'NONE', #2943, .T. ) ;
#7101 = EDGE_CURVE ( 'NONE', #1578, #1, #6878, .T. ) ;
#7102 = VECTOR ( 'NONE', #926, 1000.000000000000000 ) ;
#7103 = COLOUR_RGB ( '',0.7921568627450980005, 0.8196078431372548767, 0.9333333333333333481 ) ;
#7104 = AXIS2_PLACEMENT_3D ( 'NONE', #632, #3157, #3086 ) ;
#7105 = ORIENTED_EDGE ( 'NONE', *, *, #237, .F. ) ;
#7106 = AXIS2_PLACEMENT_3D ( 'NONE', #2815, #3413, #2168 ) ;
#7107 = MECHANICAL_DESIGN_GEOMETRIC_PRESENTATION_REPRESENTATION (  '', ( #6085 ), #7245 ) ;
#7108 = CIRCLE ( 'NONE', #51, 32.75000000000000000 ) ;
#7109 = DIRECTION ( 'NONE',  ( 1.000000000000000000, 0.000000000000000000, -0.000000000000000000 ) ) ;
#7110 = CARTESIAN_POINT ( 'NONE',  ( 75.00000000000000000, 10.56842436860067735, 0.000000000000000000 ) ) ;
#7111 = DIRECTION ( 'NONE',  ( 0.000000000000000000, -0.000000000000000000, -1.000000000000000000 ) ) ;
#7112 = CARTESIAN_POINT ( 'NONE',  ( 187.5000000000000000, 0.000000000000000000, 0.000000000000000000 ) ) ;
#7113 = CARTESIAN_POINT ( 'NONE',  ( 52.50000000000000711, 79.24999999999987210, 130.0000000000000000 ) ) ;
#7114 = CIRCLE ( 'NONE', #1724, 13.00000000000000178 ) ;
#7115 = EDGE_CURVE ( 'NONE', #6373, #5450, #2803, .T. ) ;
#7116 = CARTESIAN_POINT ( 'NONE',  ( 296.6025403784439050, 0.000000000000000000, 12.50000000000000000 ) ) ;
#7117 = ORIENTED_EDGE ( 'NONE', *, *, #5420, .F. ) ;
#7118 = CARTESIAN_POINT ( 'NONE',  ( 232.4759526419164217, 243.7500000000000000, 12.50000000000000000 ) ) ;
#7119 = DIRECTION ( 'NONE',  ( 1.000000000000000000, 0.000000000000000000, 0.000000000000000000 ) ) ;
#7121 = FACE_OUTER_BOUND ( 'NONE', #4206, .T. ) ;
#7120 = AXIS2_PLACEMENT_3D ( 'NONE', #4194, #7293, #1792 ) ;
#7122 = DIRECTION ( 'NONE',  ( -0.000000000000000000, -0.000000000000000000, -1.000000000000000000 ) ) ;
#7123 = ORIENTED_EDGE ( 'NONE', *, *, #7621, .T. ) ;
#7124 = PRODUCT_DEFINITION_CONTEXT ( 'detailed design', #3731, 'design' ) ;
#7125 = VECTOR ( 'NONE', #2068, 1000.000000000000227 ) ;
#7126 = ORIENTED_EDGE ( 'NONE', *, *, #2877, .T. ) ;
#7127 = SHAPE_REPRESENTATION_RELATIONSHIP ( 'NONE' , 'NONE' ,  #2908, #4209 ) ;
#7128 = ORIENTED_EDGE ( 'NONE', *, *, #6553, .F. ) ;
#7129 = DIRECTION ( 'NONE',  ( 0.000000000000000000, 0.000000000000000000, 1.000000000000000000 ) ) ;
#7130 = CARTESIAN_POINT ( 'NONE',  ( 412.5000000000001137, 217.5000000000000000, 20.00000000000000000 ) ) ;
#7131 = EDGE_LOOP ( 'NONE', ( #4404, #7652, #7182, #5897, #7259, #4865, #6479, #7703, #6322, #7265, #6338, #1318, #3089, #2561, #2092, #1697, #6091, #4416, #1077, #2978, #4424, #2758, #5913, #764 ) ) ;
#7132 = CARTESIAN_POINT ( 'NONE',  ( 0.7190441502950423169, -5.595828947448873159, 0.000000000000000000 ) ) ;
#7133 = LINE ( 'NONE', #7774, #1340 ) ;
#7134 = PRODUCT_DEFINITION_SHAPE ( 'NONE', 'NONE',  #7919 ) ;
#7135 = EDGE_LOOP ( 'NONE', ( #3536, #5689, #6563, #7336, #2486, #7562, #4147, #1915, #4472, #629, #7441, #3918 ) ) ;
#7136 = AXIS2_PLACEMENT_3D ( 'NONE', #2181, #1023, #3347 ) ;
#7137 = DIRECTION ( 'NONE',  ( -0.000000000000000000, -0.000000000000000000, -1.000000000000000000 ) ) ;
#7138 = ORIENTED_EDGE ( 'NONE', *, *, #6623, .T. ) ;
#7139 = CARTESIAN_POINT ( 'NONE',  ( -17.50000000000000355, 0.000000000000000000, 92.50000000000000000 ) ) ;
#7140 = ORIENTED_EDGE ( 'NONE', *, *, #4971, .T. ) ;
#7141 = ADVANCED_FACE ( 'NONE', ( #2621 ), #5058, .F. ) ;
#7142 = CARTESIAN_POINT ( 'NONE',  ( -49.28095584970496645, -62.29455879088143888, 0.000000000000000000 ) ) ;
#7143 = LINE ( 'NONE', #4088, #4282 ) ;
#7144 = AXIS2_PLACEMENT_3D ( 'NONE', #7751, #2372, #6700 ) ;
#7145 = EDGE_CURVE ( 'NONE', #6889, #7297, #2934, .T. ) ;
#7146 = ORIENTED_EDGE ( 'NONE', *, *, #7115, .F. ) ;
#7147 = EDGE_LOOP ( 'NONE', ( #3830, #7402, #2894, #5821 ) ) ;
#7148 = EDGE_CURVE ( 'NONE', #5402, #7529, #5753, .T. ) ;
#7149 = AXIS2_PLACEMENT_3D ( 'NONE', #5085, #6335, #7502 ) ;
#7150 = EDGE_CURVE ( 'NONE', #5007, #5001, #2743, .T. ) ;
#7151 = DIRECTION ( 'NONE',  ( 0.000000000000000000, -0.000000000000000000, -1.000000000000000000 ) ) ;
#7152 = DIRECTION ( 'NONE',  ( 0.000000000000000000, 0.000000000000000000, -1.000000000000000000 ) ) ;
#7153 = DIRECTION ( 'NONE',  ( 1.000000000000000000, 0.000000000000000000, 0.000000000000000000 ) ) ;
#7154 = CARTESIAN_POINT ( 'NONE',  ( 42.50000000000000000, 42.50000000000003553, 12.50000000000000000 ) ) ;
#7155 = DIRECTION ( 'NONE',  ( -1.000000000000000000, 0.000000000000000000, 0.000000000000000000 ) ) ;
#7156 = VECTOR ( 'NONE', #3370, 1000.000000000000000 ) ;
#7157 = VECTOR ( 'NONE', #465, 1000.000000000000000 ) ;
#7158 = DIRECTION ( 'NONE',  ( 0.000000000000000000, 0.000000000000000000, 1.000000000000000000 ) ) ;
#7159 = CARTESIAN_POINT ( 'NONE',  ( 257.3507467850104717, 194.6990734970208337, 252.0932327501082568 ) ) ;
#7160 = VERTEX_POINT ( 'NONE', #4136 ) ;
#7161 = AXIS2_PLACEMENT_3D ( 'NONE', #137, #6995, #1973 ) ;
#7162 = DIRECTION ( 'NONE',  ( 1.000000000000000000, 0.000000000000000000, 0.000000000000000000 ) ) ;
#7163 = DIRECTION ( 'NONE',  ( -0.5000000000000000000, -0.8660254037844385966, 0.000000000000000000 ) ) ;
#7164 = VECTOR ( 'NONE', #4535, 1000.000000000000000 ) ;
#7165 = FACE_OUTER_BOUND ( 'NONE', #2450, .T. ) ;
#7166 = EDGE_CURVE ( 'NONE', #2585, #1234, #5673, .T. ) ;
#7167 = DIRECTION ( 'NONE',  ( 1.000000000000000000, 0.000000000000000000, 0.000000000000000000 ) ) ;
#7168 = ORIENTED_EDGE ( 'NONE', *, *, #2180, .T. ) ;
#7169 = CIRCLE ( 'NONE', #2545, 24.99999998367932719 ) ;
#7170 = ORIENTED_EDGE ( 'NONE', *, *, #1504, .T. ) ;
#7171 = CIRCLE ( 'NONE', #372, 30.00000000000000000 ) ;
#7172 = ORIENTED_EDGE ( 'NONE', *, *, #4645, .F. ) ;
#7173 =( NAMED_UNIT ( * ) PLANE_ANGLE_UNIT ( ) SI_UNIT ( $, .RADIAN. ) );
#7174 = ORIENTED_EDGE ( 'NONE', *, *, #6606, .T. ) ;
#7175 = CYLINDRICAL_SURFACE ( 'NONE', #3285, 5.000000000000000000 ) ;
#7176 = FACE_OUTER_BOUND ( 'NONE', #7262, .T. ) ;
#7177 = ORIENTED_EDGE ( 'NONE', *, *, #4386, .F. ) ;
#7178 = SURFACE_STYLE_FILL_AREA ( #5927 ) ;
#7179 = CARTESIAN_POINT ( 'NONE',  ( 0.000000000000000000, -25.00000000000000000, 25.00000000000000000 ) ) ;
#7180 = ORIENTED_EDGE ( 'NONE', *, *, #928, .F. ) ;
#7181 = DIRECTION ( 'NONE',  ( 0.000000000000000000, 1.000000000000000000, -0.000000000000000000 ) ) ;
#7182 = ORIENTED_EDGE ( 'NONE', *, *, #5514, .F. ) ;
#7183 = ADVANCED_FACE ( 'NONE', ( #331 ), #2308, .F. ) ;
#7184 = DIRECTION ( 'NONE',  ( 1.000000000000000000, 0.000000000000000000, 0.000000000000000000 ) ) ;
#7185 = EDGE_LOOP ( 'NONE', ( #2630, #408, #2107, #3346 ) ) ;
#7186 = DIRECTION ( 'NONE',  ( -0.000000000000000000, -0.000000000000000000, -1.000000000000000000 ) ) ;
#7187 = CYLINDRICAL_SURFACE ( 'NONE', #306, 12.50000000000001066 ) ;
#7188 = VERTEX_POINT ( 'NONE', #1660 ) ;
#7189 = ADVANCED_FACE ( 'NONE', ( #505, #7199 ), #7796, .F. ) ;
#7190 = EDGE_LOOP ( 'NONE', ( #5640, #5488, #5940, #1839, #2564, #211, #1272, #7242, #3320, #2931, #310, #5804 ) ) ;
#7191 = EDGE_CURVE ( 'NONE', #7188, #4785, #5912, .T. ) ;
#7192 = CARTESIAN_POINT ( 'NONE',  ( -12.50000000000000000, -24.99999999999999645, -3.235013004037443297E-15 ) ) ;
#7193 = CARTESIAN_POINT ( 'NONE',  ( 25.00000000000000000, 0.000000000000000000, 0.000000000000000000 ) ) ;
#7194 = LINE ( 'NONE', #5416, #146 ) ;
#7195 = CARTESIAN_POINT ( 'NONE',  ( -13.00000000000000178, 1.592040838891559293E-15, 0.5000000000000004441 ) ) ;
#7196 = CARTESIAN_POINT ( 'NONE',  ( 387.0648300283518211, 19.73070161726337446, -3.295910870315892804 ) ) ;
#7197 = ADVANCED_FACE ( 'NONE', ( #6590 ), #7235, .F. ) ;
#7198 = ORIENTED_EDGE ( 'NONE', *, *, #5725, .T. ) ;
#7199 = FACE_OUTER_BOUND ( 'NONE', #4718, .T. ) ;
#7200 = DIRECTION ( 'NONE',  ( 1.000000000000000000, -4.789593822244094799E-16, -4.789593822244094799E-16 ) ) ;
#7201 = ORIENTED_EDGE ( 'NONE', *, *, #579, .T. ) ;
#7202 = CARTESIAN_POINT ( 'NONE',  ( 0.000000000000000000, 0.000000000000000000, 45.00000000000000000 ) ) ;
#7203 = FACE_OUTER_BOUND ( 'NONE', #4970, .T. ) ;
#7204 = FACE_OUTER_BOUND ( 'NONE', #2963, .T. ) ;
#7205 = EDGE_LOOP ( 'NONE', ( #5379, #3546, #6295, #2958 ) ) ;
#7206 = PRODUCT_DEFINITION_SHAPE ( 'NONE', 'NONE',  #7930 ) ;
#7207 = ADVANCED_FACE ( 'NONE', ( #6471 ), #1695, .T. ) ;
#7208 = ORIENTED_EDGE ( 'NONE', *, *, #6409, .F. ) ;
#7209 = VERTEX_POINT ( 'NONE', #3471 ) ;
#7210 = EDGE_LOOP ( 'NONE', ( #7086, #799, #4639, #4237 ) ) ;
#7211 = CARTESIAN_POINT ( 'NONE',  ( 0.000000000000000000, 0.000000000000000000, 200.0000000000000000 ) ) ;
#7212 = DIRECTION ( 'NONE',  ( 1.000000000000000000, 0.000000000000000000, 0.000000000000000000 ) ) ;
#7213 = ORIENTED_EDGE ( 'NONE', *, *, #810, .T. ) ;
#7214 = CYLINDRICAL_SURFACE ( 'NONE', #6861, 12.50000000000001066 ) ;
#7215 = VERTEX_POINT ( 'NONE', #6555 ) ;
#7216 = ADVANCED_FACE ( 'NONE', ( #1613 ), #4016, .T. ) ;
#7217 = DIRECTION ( 'NONE',  ( -1.000000000000000000, 0.000000000000000000, 0.000000000000000000 ) ) ;
#7218 = ORIENTED_EDGE ( 'NONE', *, *, #4236, .F. ) ;
#7219 = CARTESIAN_POINT ( 'NONE',  ( 362.9446671282877332, -19.72489609666084576, 3.330011984645298462 ) ) ;
#7220 = VERTEX_POINT ( 'NONE', #1094 ) ;
#7221 = DIRECTION ( 'NONE',  ( 1.000000000000000000, 0.000000000000000000, 0.000000000000000000 ) ) ;
#7222 = FACE_OUTER_BOUND ( 'NONE', #6210, .T. ) ;
#7223 = ORIENTED_EDGE ( 'NONE', *, *, #776, .T. ) ;
#7224 = CIRCLE ( 'NONE', #1199, 15.00000000000000000 ) ;
#7225 = ORIENTED_EDGE ( 'NONE', *, *, #374, .F. ) ;
#7226 = DIRECTION ( 'NONE',  ( -1.000000000000000000, -0.000000000000000000, -0.000000000000000000 ) ) ;
#7227 = FACE_OUTER_BOUND ( 'NONE', #3205, .T. ) ;
#7228 = DIRECTION ( 'NONE',  ( 0.000000000000000000, 0.000000000000000000, 1.000000000000000000 ) ) ;
#7229 = AXIS2_PLACEMENT_3D ( 'NONE', #246, #282, #6418 ) ;
#7230 = VECTOR ( 'NONE', #4223, 1000.000000000000000 ) ;
#7231 = CARTESIAN_POINT ( 'NONE',  ( -37.49999999999995026, 47.50000000000009237, 130.0000000000000000 ) ) ;
#7232 = CARTESIAN_POINT ( 'NONE',  ( 382.3165647940696203, 17.23925164521633846, -10.14275924251023220 ) ) ;
#7233 = AXIS2_PLACEMENT_3D ( 'NONE', #4976, #7466, #3251 ) ;
#7234 = AXIS2_PLACEMENT_3D ( 'NONE', #7447, #5763, #2023 ) ;
#7235 = CYLINDRICAL_SURFACE ( 'NONE', #7284, 12.50000000000000000 ) ;
#7236 = APPLICATION_PROTOCOL_DEFINITION ( 'draft international standard', 'automotive_design', 1998, #2591 ) ;
#7237 = DIRECTION ( 'NONE',  ( 1.000000000000000000, 0.000000000000000000, 0.000000000000000000 ) ) ;
#7238 = DIRECTION ( 'NONE',  ( 0.000000000000000000, 0.000000000000000000, -1.000000000000000000 ) ) ;
#7239 = DIRECTION ( 'NONE',  ( 0.000000000000000000, 0.000000000000000000, 1.000000000000000000 ) ) ;
#7240 = EDGE_CURVE ( 'NONE', #6431, #4276, #3544, .T. ) ;
#7241 = CYLINDRICAL_SURFACE ( 'NONE', #3021, 37.50000000000003553 ) ;
#7242 = ORIENTED_EDGE ( 'NONE', *, *, #7264, .T. ) ;
#7243 = EDGE_CURVE ( 'NONE', #2325, #6102, #6780, .T. ) ;
#7244 = VECTOR ( 'NONE', #5892, 1000.000000000000000 ) ;
#7245 =( GEOMETRIC_REPRESENTATION_CONTEXT ( 3 ) GLOBAL_UNCERTAINTY_ASSIGNED_CONTEXT ( ( #5765 ) ) GLOBAL_UNIT_ASSIGNED_CONTEXT ( ( #1543, #2225, #6524 ) ) REPRESENTATION_CONTEXT ( 'NONE', 'WORKASPACE' ) );
#7246 = EDGE_CURVE ( 'NONE', #1141, #5747, #5101, .T. ) ;
#7247 = ORIENTED_EDGE ( 'NONE', *, *, #911, .T. ) ;
#7248 = VERTEX_POINT ( 'NONE', #2343 ) ;
#7249 = AXIS2_PLACEMENT_3D ( 'NONE', #5418, #3543, #7863 ) ;
#7250 = VERTEX_POINT ( 'NONE', #417 ) ;
#7251 = EDGE_CURVE ( 'NONE', #7015, #5922, #7169, .T. ) ;
#7252 =( LENGTH_UNIT ( ) NAMED_UNIT ( * ) SI_UNIT ( .MILLI., .METRE. ) );
#7253 = FACE_OUTER_BOUND ( 'NONE', #339, .T. ) ;
#7254 = DIRECTION ( 'NONE',  ( 0.000000000000000000, 0.000000000000000000, 1.000000000000000000 ) ) ;
#7255 = EDGE_LOOP ( 'NONE', ( #1455, #2961, #6567, #59 ) ) ;
#7256 = DIRECTION ( 'NONE',  ( -0.000000000000000000, -0.000000000000000000, -1.000000000000000000 ) ) ;
#7257 = VECTOR ( 'NONE', #301, 1000.000000000000000 ) ;
#7258 = CARTESIAN_POINT ( 'NONE',  ( 199.9999999999998863, 225.0000000000000284, 0.000000000000000000 ) ) ;
#7259 = ORIENTED_EDGE ( 'NONE', *, *, #1207, .F. ) ;
#7260 = CARTESIAN_POINT ( 'NONE',  ( 363.1903364394804044, -19.57571528166833019, 4.117265725333339788 ) ) ;
#7261 = CIRCLE ( 'NONE', #1483, 25.00000003264134918 ) ;
#7262 = EDGE_LOOP ( 'NONE', ( #6529, #1710, #178, #4561 ) ) ;
#7263 = CARTESIAN_POINT ( 'NONE',  ( 400.0000000000000000, 0.000000000000000000, 0.000000000000000000 ) ) ;
#7264 = EDGE_CURVE ( 'NONE', #308, #1401, #5871, .T. ) ;
#7265 = ORIENTED_EDGE ( 'NONE', *, *, #2877, .F. ) ;
#7266 = VERTEX_POINT ( 'NONE', #2177 ) ;
#7267 = LINE ( 'NONE', #2980, #496 ) ;
#7268 = DIRECTION ( 'NONE',  ( -0.000000000000000000, 0.000000000000000000, 1.000000000000000000 ) ) ;
#7269 = DIRECTION ( 'NONE',  ( 1.000000000000000000, 0.000000000000000000, 0.000000000000000000 ) ) ;
#7271 = DIRECTION ( 'NONE',  ( 0.000000000000000000, 1.000000000000000000, -0.000000000000000000 ) ) ;
#7270 = AXIS2_PLACEMENT_3D ( 'NONE', #6063, #1169, #1126 ) ;
#7272 = CARTESIAN_POINT ( 'NONE',  ( 12.50000000000000355, 0.000000000000000000, 0.000000000000000000 ) ) ;
#7273 = DIRECTION ( 'NONE',  ( -0.000000000000000000, -0.000000000000000000, -1.000000000000000000 ) ) ;
#7274 = AXIS2_PLACEMENT_3D ( 'NONE', #78, #6103, #4887 ) ;
#7275 = CARTESIAN_POINT ( 'NONE',  ( -9.381941874331415576, 16.25000000000000000, 0.000000000000000000 ) ) ;
#7276 = PRODUCT_CONTEXT ( 'NONE', #4943, 'mechanical' ) ;
#7277 = LINE ( 'NONE', #6072, #5851 ) ;
#7278 = FACE_OUTER_BOUND ( 'NONE', #6133, .T. ) ;
#7279 = FACE_BOUND ( 'NONE', #357, .T. ) ;
#7280 = CARTESIAN_POINT ( 'NONE',  ( 32.53766565774834163, -18.78563002630307111, 12.50000000000000000 ) ) ;
#7281 = ORIENTED_EDGE ( 'NONE', *, *, #2491, .T. ) ;
#7282 = PRODUCT_DEFINITION_CONTEXT ( 'detailed design', #6033, 'design' ) ;
#7283 = ORIENTED_EDGE ( 'NONE', *, *, #1501, .T. ) ;
#7284 = AXIS2_PLACEMENT_3D ( 'NONE', #4695, #4061, #1570 ) ;
#7285 = EDGE_CURVE ( 'NONE', #2331, #7745, #3575, .T. ) ;
#7286 = AXIS2_PLACEMENT_3D ( 'NONE', #4337, #5053, #7508 ) ;
#7287 = EDGE_LOOP ( 'NONE', ( #3867, #3884, #2557, #3631 ) ) ;
#7288 = CARTESIAN_POINT ( 'NONE',  ( 0.000000000000000000, 137.4999999999999716, 12.50000000000000000 ) ) ;
#7289 = CARTESIAN_POINT ( 'NONE',  ( -25.00000000000000000, 0.000000000000000000, 0.000000000000000000 ) ) ;
#7290 = DIRECTION ( 'NONE',  ( 0.000000000000000000, -0.000000000000000000, 1.000000000000000000 ) ) ;
#7291 = EDGE_CURVE ( 'NONE', #2150, #3303, #3828, .T. ) ;
#7292 = EDGE_LOOP ( 'NONE', ( #867, #5369, #2274, #4305 ) ) ;
#7293 = DIRECTION ( 'NONE',  ( 0.000000000000000000, 1.000000000000000000, 0.000000000000000000 ) ) ;
#7294 = VECTOR ( 'NONE', #5120, 1000.000000000000114 ) ;
#7295 = AXIS2_PLACEMENT_3D ( 'NONE', #6786, #3745, #6187 ) ;
#7296 = EDGE_CURVE ( 'NONE', #2321, #5516, #3288, .T. ) ;
#7297 = VERTEX_POINT ( 'NONE', #4099 ) ;
#7298 = LINE ( 'NONE', #5449, #377 ) ;
#7299 = ORIENTED_EDGE ( 'NONE', *, *, #2971, .T. ) ;
#7300 = AXIS2_PLACEMENT_3D ( 'NONE', #5368, #558, #3643 ) ;
#7301 = CARTESIAN_POINT ( 'NONE',  ( 369.7712349971211552, -16.46093790404528789, 11.36110438390628197 ) ) ;
#7302 = AXIS2_PLACEMENT_3D ( 'NONE', #526, #7783, #5857 ) ;
#7303 = VERTEX_POINT ( 'NONE', #5543 ) ;
#7304 = DIRECTION ( 'NONE',  ( -0.000000000000000000, 0.000000000000000000, 1.000000000000000000 ) ) ;
#7305 = DIRECTION ( 'NONE',  ( 0.000000000000000000, -1.000000000000000000, 0.000000000000000000 ) ) ;
#7306 = EDGE_LOOP ( 'NONE', ( #7422, #2467 ) ) ;
#7307 = EDGE_LOOP ( 'NONE', ( #514, #6996, #5033, #7695 ) ) ;
#7308 = EDGE_CURVE ( 'NONE', #6609, #5012, #11, .T. ) ;
#7309 = CARTESIAN_POINT ( 'NONE',  ( 0.000000000000000000, 0.000000000000000000, 45.00000000000000000 ) ) ;
#7310 = DIRECTION ( 'NONE',  ( 1.000000000000000000, 0.000000000000000000, 0.000000000000000000 ) ) ;
#7311 = DIRECTION ( 'NONE',  ( 1.000000000000000000, 0.000000000000000000, -0.000000000000000000 ) ) ;
#7312 = CARTESIAN_POINT ( 'NONE',  ( 12.50000000000000000, 0.000000000000000000, 2.000000000000001776 ) ) ;
#7313 = DIRECTION ( 'NONE',  ( -0.5000000000000000000, -0.8660254037844385966, 0.000000000000000000 ) ) ;
#7314 = CARTESIAN_POINT ( 'NONE',  ( 387.4182085429678750, 19.94855572367474750, -1.655112461855906769 ) ) ;
#7315 = EDGE_CURVE ( 'NONE', #3577, #260, #4335, .T. ) ;
#7316 = DIRECTION ( 'NONE',  ( 4.789677997474691297E-16, -1.000000000000000000, 0.000000000000000000 ) ) ;
#7317 = DIRECTION ( 'NONE',  ( -0.000000000000000000, -0.000000000000000000, -1.000000000000000000 ) ) ;
#7318 = FACE_OUTER_BOUND ( 'NONE', #6879, .T. ) ;
#7319 = DIRECTION ( 'NONE',  ( 1.000000000000000000, 0.000000000000000000, 0.000000000000000000 ) ) ;
#7320 =( REPRESENTATION_RELATIONSHIP ('NONE','NONE', #6292, #2908 ) REPRESENTATION_RELATIONSHIP_WITH_TRANSFORMATION ( #3785 )SHAPE_REPRESENTATION_RELATIONSHIP( ) );
#7321 = FACE_OUTER_BOUND ( 'NONE', #1045, .T. ) ;
#7322 = ORIENTED_EDGE ( 'NONE', *, *, #4966, .F. ) ;
#7323 = EDGE_CURVE ( 'NONE', #1302, #7538, #3847, .T. ) ;
#7324 = ORIENTED_EDGE ( 'NONE', *, *, #1491, .F. ) ;
#7325 = DIRECTION ( 'NONE',  ( 1.000000000000000000, 0.000000000000000000, 0.000000000000000000 ) ) ;
#7326 = PLANE ( 'NONE',  #4707 ) ;
#7327 = DIRECTION ( 'NONE',  ( 1.000000000000000000, 0.000000000000000000, 0.000000000000000000 ) ) ;
#7328 = FACE_OUTER_BOUND ( 'NONE', #280, .T. ) ;
#7329 = ORIENTED_EDGE ( 'NONE', *, *, #1693, .T. ) ;
#7330 = DIRECTION ( 'NONE',  ( -1.000000000000000000, 0.000000000000000000, 0.000000000000000000 ) ) ;
#7331 = PRODUCT_RELATED_PRODUCT_CATEGORY ( 'part', '', ( #3417 ) ) ;
#7332 = EDGE_CURVE ( 'NONE', #2517, #756, #618, .T. ) ;
#7333 = PRODUCT_DEFINITION_SHAPE ( 'NONE', 'NONE',  #7929 ) ;
#7334 = ORIENTED_EDGE ( 'NONE', *, *, #5562, .F. ) ;
#7335 = CARTESIAN_POINT ( 'NONE',  ( 375.0000000000000000, 15.61249499599599488, -12.50000000000000000 ) ) ;
#7336 = ORIENTED_EDGE ( 'NONE', *, *, #4359, .F. ) ;
#7337 = FACE_BOUND ( 'NONE', #7683, .T. ) ;
#7338 = ORIENTED_EDGE ( 'NONE', *, *, #3171, .F. ) ;
#7339 = EDGE_CURVE ( 'NONE', #4682, #6684, #7867, .T. ) ;
#7340 = CARTESIAN_POINT ( 'NONE',  ( 162.5000000000000000, 37.50000000000006395, 12.50000000000000000 ) ) ;
#7341 = ADVANCED_FACE ( 'NONE', ( #7498 ), #4719, .T. ) ;
#7342 = VERTEX_POINT ( 'NONE', #3071 ) ;
#7343 = ORIENTED_EDGE ( 'NONE', *, *, #1766, .F. ) ;
#7344 = VERTEX_POINT ( 'NONE', #2420 ) ;
#7345 = DIRECTION ( 'NONE',  ( -0.000000000000000000, 0.000000000000000000, 1.000000000000000000 ) ) ;
#7346 = ADVANCED_FACE ( 'NONE', ( #4439 ), #6069, .T. ) ;
#7347 = CARTESIAN_POINT ( 'NONE',  ( -12.50000000000000000, 0.000000000000000000, 0.000000000000000000 ) ) ;
#7348 = CARTESIAN_POINT ( 'NONE',  ( 4.000000000000004441, 0.000000000000000000, 0.000000000000000000 ) ) ;
#7349 = CARTESIAN_POINT ( 'NONE',  ( 42.50000000000000711, 177.5000000000000000, 12.65877081724072362 ) ) ;
#7350 = DIRECTION ( 'NONE',  ( 1.000000000000000000, 2.960594732333750117E-15, -0.000000000000000000 ) ) ;
#7351 = CLOSED_SHELL ( 'NONE', ( #4573, #1671, #2233, #6833, #4251, #7729, #5919, #1951, #6110, #6985, #3046, #7039, #3898, #6845, #7183, #6552, #1659, #317, #6994, #5893, #1201, #6156, #2093, #4585, #1838, #2783, #5726, #5059, #6895, #79, #6992, #7189, #1813, #5056, #425, #455, #3271, #3079, #7503, #6613, #531, #1986, #6897, #5374, #1107, #6946, #7197, #3441, #7668, #1880, #2731, #6794, #7843, #61, #834, #1123, #7659, #5273, #2882, #5377, #1252, #3952, #3318, #3913, #3689, #3361, #5050, #169, #7433, #219, #429, #7141, #2439, #26 ) ) ;
#7352 = DIRECTION ( 'NONE',  ( -0.000000000000000000, -0.000000000000000000, -1.000000000000000000 ) ) ;
#7353 = AXIS2_PLACEMENT_3D ( 'NONE', #7154, #7709, #1490 ) ;
#7354 = PRODUCT_CONTEXT ( 'NONE', #1921, 'mechanical' ) ;
#7355 = VECTOR ( 'NONE', #7327, 1000.000000000000000 ) ;
#7356 = PLANE ( 'NONE',  #1109 ) ;
#7357 = DIRECTION ( 'NONE',  ( -0.000000000000000000, -0.000000000000000000, -1.000000000000000000 ) ) ;
#7358 = DIRECTION ( 'NONE',  ( 1.000000000000000000, 0.000000000000000000, -0.000000000000000000 ) ) ;
#7359 = CARTESIAN_POINT ( 'NONE',  ( 187.4999999999998863, 225.0000000000000284, 12.50000000000000000 ) ) ;
#7360 = EDGE_CURVE ( 'NONE', #3018, #1497, #885, .T. ) ;
#7361 = AXIS2_PLACEMENT_3D ( 'NONE', #5901, #2857, #2771 ) ;
#7362 = VERTEX_POINT ( 'NONE', #540 ) ;
#7363 = ORIENTED_EDGE ( 'NONE', *, *, #1311, .F. ) ;
#7364 = SURFACE_STYLE_FILL_AREA ( #516 ) ;
#7365 = CARTESIAN_POINT ( 'NONE',  ( -12.50000000000000000, 0.000000000000000000, 12.50000000000000000 ) ) ;
#7367 = CARTESIAN_POINT ( 'NONE',  ( 338.3083524847280614, 75.00000000000005684, 168.7439889854708213 ) ) ;
#7366 = AXIS2_PLACEMENT_3D ( 'NONE', #3282, #351, #5733 ) ;
#7368 = CIRCLE ( 'NONE', #5310, 17.50000000000000355 ) ;
#7369 = LINE ( 'NONE', #1790, #44 ) ;
#7370 = VERTEX_POINT ( 'NONE', #194 ) ;
#7371 = LINE ( 'NONE', #104, #6476 ) ;
#7372 = UNCERTAINTY_MEASURE_WITH_UNIT (LENGTH_MEASURE( 1.000000000000000082E-05 ), #2445, 'distance_accuracy_value', 'NONE');
#7373 = VECTOR ( 'NONE', #4755, 1000.000000000000114 ) ;
#7374 = EDGE_LOOP ( 'NONE', ( #5676, #4227 ) ) ;
#7375 = CARTESIAN_POINT ( 'NONE',  ( 362.5018422615490294, 19.99884858813039301, -0.8730781214943976742 ) ) ;
#7376 = ORIENTED_EDGE ( 'NONE', *, *, #4737, .F. ) ;
#7377 = CARTESIAN_POINT ( 'NONE',  ( 375.0000000000000000, -15.61249499599599488, -12.50000000000000000 ) ) ;
#7378 = ORIENTED_EDGE ( 'NONE', *, *, #1420, .T. ) ;
#7379 =( NAMED_UNIT ( * ) PLANE_ANGLE_UNIT ( ) SI_UNIT ( $, .RADIAN. ) );
#7380 = VECTOR ( 'NONE', #5813, 1000.000000000000000 ) ;
#7381 = DIRECTION ( 'NONE',  ( 1.000000000000000000, 0.000000000000000000, 0.000000000000000000 ) ) ;
#7382 = VERTEX_POINT ( 'NONE', #2602 ) ;
#7383=STYLED_ITEM('',(#7948),#4034);
#7384 = ORIENTED_EDGE ( 'NONE', *, *, #147, .F. ) ;
#7385 = ADVANCED_FACE ( 'NONE', ( #5041 ), #4895, .T. ) ;
#7386 = ORIENTED_EDGE ( 'NONE', *, *, #7291, .T. ) ;
#7387 = FACE_OUTER_BOUND ( 'NONE', #3567, .T. ) ;
#7388 = CARTESIAN_POINT ( 'NONE',  ( 385.7978869038915946, -18.97902931052027142, -6.348195341973490891 ) ) ;
#7389 = DIRECTION ( 'NONE',  ( 0.000000000000000000, 0.000000000000000000, 1.000000000000000000 ) ) ;
#7390 = CARTESIAN_POINT ( 'NONE',  ( 296.6025403784437913, 0.000000000000000000, 12.50000000000000000 ) ) ;
#7391 = EDGE_CURVE ( 'NONE', #3478, #2517, #1274, .T. ) ;
#7392 = CARTESIAN_POINT ( 'NONE',  ( -6.945033096338293890E-14, 144.9999999999998295, 5.000000000000000000 ) ) ;
#7393 = AXIS2_PLACEMENT_3D ( 'NONE', #1105, #7325, #1748 ) ;
#7394 = EDGE_CURVE ( 'NONE', #3133, #5735, #4460, .T. ) ;
#7395 = VECTOR ( 'NONE', #7714, 1000.000000000000114 ) ;
#7396 = APPLICATION_PROTOCOL_DEFINITION ( 'draft international standard', 'automotive_design', 1998, #6798 ) ;
#7397 = DIRECTION ( 'NONE',  ( 0.000000000000000000, 0.000000000000000000, -1.000000000000000000 ) ) ;
#7398 = CYLINDRICAL_SURFACE ( 'NONE', #7286, 12.50000000000000000 ) ;
#7399 = CARTESIAN_POINT ( 'NONE',  ( 326.6025403784438481, 150.0000000000000568, 125.0000000000000000 ) ) ;
#7400 = CARTESIAN_POINT ( 'NONE',  ( 0.000000000000000000, 0.000000000000000000, 12.50000000000000000 ) ) ;
#7401 = AXIS2_PLACEMENT_3D ( 'NONE', #4336, #1369, #1330 ) ;
#7402 = ORIENTED_EDGE ( 'NONE', *, *, #4728, .F. ) ;
#7403 = EDGE_LOOP ( 'NONE', ( #1670, #6437 ) ) ;
#7404 = EDGE_CURVE ( 'NONE', #3018, #6617, #5696, .T. ) ;
#7405 = DIRECTION ( 'NONE',  ( -0.000000000000000000, -0.000000000000000000, -1.000000000000000000 ) ) ;
#7406 = LINE ( 'NONE', #778, #3438 ) ;
#7407 = AXIS2_PLACEMENT_3D ( 'NONE', #7857, #4851, #1806 ) ;
#7408 = DIRECTION ( 'NONE',  ( 1.000000000000000000, 0.000000000000000000, 0.000000000000000000 ) ) ;
#7409 = DIRECTION ( 'NONE',  ( -0.000000000000000000, -0.000000000000000000, -1.000000000000000000 ) ) ;
#7410 = EDGE_LOOP ( 'NONE', ( #6525, #2851, #6612, #3246, #5531 ) ) ;
#7411 = DIRECTION ( 'NONE',  ( -4.789677997474686366E-16, -1.000000000000000000, -0.000000000000000000 ) ) ;
#7412 = CIRCLE ( 'NONE', #3185, 12.50000000000001776 ) ;
#7413 = EDGE_LOOP ( 'NONE', ( #2444, #2878, #224, #3212 ) ) ;
#7414 = CARTESIAN_POINT ( 'NONE',  ( 366.4564998757169292, 17.79554561421092984, 9.133253117746194860 ) ) ;
#7415 = ORIENTED_EDGE ( 'NONE', *, *, #2959, .F. ) ;
#7416 = LINE ( 'NONE', #3165, #466 ) ;
#7417 = ORIENTED_EDGE ( 'NONE', *, *, #1649, .T. ) ;
#7418 = AXIS2_PLACEMENT_3D ( 'NONE', #1133, #7905, #3623 ) ;
#7419 = DIRECTION ( 'NONE',  ( -0.000000000000000000, -0.000000000000000000, -1.000000000000000000 ) ) ;
#7420 = AXIS2_PLACEMENT_3D ( 'NONE', #6988, #1533, #3974 ) ;
#7421 = CARTESIAN_POINT ( 'NONE',  ( -17.50000000000000355, 0.000000000000000000, 75.00000000000000000 ) ) ;
#7422 = ORIENTED_EDGE ( 'NONE', *, *, #7458, .T. ) ;
#7423 = AXIS2_PLACEMENT_3D ( 'NONE', #4199, #3527, #5974 ) ;
#7424 = VECTOR ( 'NONE', #5130, 1000.000000000000000 ) ;
#7425 = ORIENTED_EDGE ( 'NONE', *, *, #1374, .T. ) ;
#7426 = ORIENTED_EDGE ( 'NONE', *, *, #525, .F. ) ;
#7427 = CARTESIAN_POINT ( 'NONE',  ( -74.28095588234631919, 0.000000000000000000, 0.000000000000000000 ) ) ;
#7428 = DIRECTION ( 'NONE',  ( 0.8886649088774987160, 0.4585571717133501424, -0.000000000000000000 ) ) ;
#7429 = DIRECTION ( 'NONE',  ( 1.000000000000000000, 0.000000000000000000, 0.000000000000000000 ) ) ;
#7430 = CARTESIAN_POINT ( 'NONE',  ( 42.50000000000000711, 182.5000000000000000, 0.000000000000000000 ) ) ;
#7431 = CARTESIAN_POINT ( 'NONE',  ( 0.000000000000000000, 0.000000000000000000, 7.500000000000000000 ) ) ;
#7432 = EDGE_CURVE ( 'NONE', #4376, #5578, #2306, .T. ) ;
#7433 = ADVANCED_FACE ( 'NONE', ( #2989 ), #5421, .F. ) ;
#7434 = APPLICATION_PROTOCOL_DEFINITION ( 'draft international standard', 'automotive_design', 1998, #3927 ) ;
#7435 = CARTESIAN_POINT ( 'NONE',  ( 20.00000000000000000, 2.449293598294706513E-15, 52.50000000000000000 ) ) ;
#7436 = CARTESIAN_POINT ( 'NONE',  ( 200.0000000000000000, 0.000000000000000000, 12.50000000000000000 ) ) ;
#7437 = CARTESIAN_POINT ( 'NONE',  ( -25.00000000000000000, 24.99999999999999289, 50.00000000000000000 ) ) ;
#7438 = CARTESIAN_POINT ( 'NONE',  ( -17.99038105676657651, 1.734723475976807094E-15, 0.000000000000000000 ) ) ;
#7439 = EDGE_CURVE ( 'NONE', #4603, #2565, #6387, .T. ) ;
#7440 = EDGE_CURVE ( 'NONE', #6592, #3133, #7806, .T. ) ;
#7441 = ORIENTED_EDGE ( 'NONE', *, *, #3986, .T. ) ;
#7442 =( NAMED_UNIT ( * ) PLANE_ANGLE_UNIT ( ) SI_UNIT ( $, .RADIAN. ) );
#7443 = ORIENTED_EDGE ( 'NONE', *, *, #5793, .F. ) ;
#7444 = PRESENTATION_STYLE_ASSIGNMENT (( #1456 ) ) ;
#7445 = LINE ( 'NONE', #3794, #6381 ) ;
#7446 = CARTESIAN_POINT ( 'NONE',  ( 12.50000000000000000, 1.530808498934191127E-15, 1.000000000000028644 ) ) ;
#7447 = CARTESIAN_POINT ( 'NONE',  ( 400.0000000000000568, 0.000000000000000000, 25.00000000000000000 ) ) ;
#7448 = EDGE_LOOP ( 'NONE', ( #7461, #1198, #2396, #4388, #3964, #6862 ) ) ;
#7449 = EDGE_CURVE ( 'NONE', #3363, #243, #2032, .T. ) ;
#7450 = FACE_OUTER_BOUND ( 'NONE', #2138, .T. ) ;
#7451 = EDGE_LOOP ( 'NONE', ( #1223, #3164, #5219, #3017 ) ) ;
#7452 = CARTESIAN_POINT ( 'NONE',  ( 363.1816593327628198, 19.58094920198549360, 4.092816503359988367 ) ) ;
#7453 = ORIENTED_EDGE ( 'NONE', *, *, #490, .F. ) ;
#7454 = DIRECTION ( 'NONE',  ( -0.000000000000000000, -0.000000000000000000, -1.000000000000000000 ) ) ;
#7455 = ORIENTED_EDGE ( 'NONE', *, *, #1897, .T. ) ;
#7456 = CARTESIAN_POINT ( 'NONE',  ( 18.76388374866283471, -1.044563157018773529E-16, 7.500000000000000000 ) ) ;
#7457 = CARTESIAN_POINT ( 'NONE',  ( 62.50000000000008527, 111.9999999999998863, 130.0000000000000000 ) ) ;
#7458 = EDGE_CURVE ( 'NONE', #1108, #4729, #1135, .T. ) ;
#7459 = ORIENTED_EDGE ( 'NONE', *, *, #1449, .F. ) ;
#7460 = ORIENTED_EDGE ( 'NONE', *, *, #414, .T. ) ;
#7461 = ORIENTED_EDGE ( 'NONE', *, *, #3168, .F. ) ;
#7462 = CARTESIAN_POINT ( 'NONE',  ( 52.50000000000000711, 177.5000000000000000, 12.50000000000000000 ) ) ;
#7463 = CARTESIAN_POINT ( 'NONE',  ( -0.000000000000000000, 177.5000000000000000, 0.000000000000000000 ) ) ;
#7464 = FACE_OUTER_BOUND ( 'NONE', #4708, .T. ) ;
#7465 = ORIENTED_EDGE ( 'NONE', *, *, #3667, .T. ) ;
#7466 = DIRECTION ( 'NONE',  ( -0.000000000000000000, -0.000000000000000000, -1.000000000000000000 ) ) ;
#7467 = SHAPE_REPRESENTATION ( 'Nut', ( #5785 ), #1293 ) ;
#7468 = PRODUCT_DEFINITION ( 'UNKNOWN', '', #6934, #1668 ) ;
#7469 = CARTESIAN_POINT ( 'NONE',  ( 187.4999999999998863, 225.0000000000000284, 12.50000000000000000 ) ) ;
#7470 = LINE ( 'NONE', #619, #5754 ) ;
#7471 = CARTESIAN_POINT ( 'NONE',  ( -10.82531754730547746, -13.74999999999999467, 7.500000000000000000 ) ) ;
#7472 = DIRECTION ( 'NONE',  ( 1.000000000000000000, 0.000000000000000000, 0.000000000000000000 ) ) ;
#7473 = ORIENTED_EDGE ( 'NONE', *, *, #2332, .T. ) ;
#7474 = TOROIDAL_SURFACE ( 'NONE', #5173, 13.00000000000000178, 0.5000000000000000000 ) ;
#7475 = CLOSED_SHELL ( 'NONE', ( #321, #7216, #2025, #3469, #4192, #2773, #1440, #6066, #2700, #7002, #274 ) ) ;
#7476 = FACE_OUTER_BOUND ( 'NONE', #2512, .T. ) ;
#7477 = ORIENTED_EDGE ( 'NONE', *, *, #3171, .T. ) ;
#7478 = EDGE_CURVE ( 'NONE', #6642, #4785, #6009, .T. ) ;
#7479 = CYLINDRICAL_SURFACE ( 'NONE', #1262, 32.75000000000001421 ) ;
#7480 = FACE_OUTER_BOUND ( 'NONE', #1337, .T. ) ;
#7481 = CARTESIAN_POINT ( 'NONE',  ( -37.49999999999997158, 1.601283208593976678E-14, 5.000000000000000000 ) ) ;
#7482 = ORIENTED_EDGE ( 'NONE', *, *, #661, .T. ) ;
#7483 = EDGE_CURVE ( 'NONE', #3721, #3479, #7032, .T. ) ;
#7484 = FACE_OUTER_BOUND ( 'NONE', #4067, .T. ) ;
#7485 = CONICAL_SURFACE ( 'NONE', #1965, 20.00000000000000000, 0.7853981633974578269 ) ;
#7486 = AXIS2_PLACEMENT_3D ( 'NONE', #83, #2534, #2608 ) ;
#7487 = EDGE_CURVE ( 'NONE', #3245, #4927, #1555, .T. ) ;
#7488 = FACE_OUTER_BOUND ( 'NONE', #1679, .T. ) ;
#7489 = AXIS2_PLACEMENT_3D ( 'NONE', #4267, #1230, #3683 ) ;
#7490 = ORIENTED_EDGE ( 'NONE', *, *, #1528, .F. ) ;
#7491 = CYLINDRICAL_SURFACE ( 'NONE', #4936, 12.50000000000000355 ) ;
#7492 = VERTEX_POINT ( 'NONE', #5197 ) ;
#7493 = CARTESIAN_POINT ( 'NONE',  ( 0.000000000000000000, 187.4999999999999432, 12.50000000000000000 ) ) ;
#7494 = CARTESIAN_POINT ( 'NONE',  ( 0.000000000000000000, 0.000000000000000000, 90.00000000000000000 ) ) ;
#7495 = VECTOR ( 'NONE', #5005, 1000.000000000000000 ) ;
#7496 = AXIS2_PLACEMENT_3D ( 'NONE', #5342, #4171, #6511 ) ;
#7497 = ORIENTED_EDGE ( 'NONE', *, *, #4852, .F. ) ;
#7498 = FACE_OUTER_BOUND ( 'NONE', #931, .T. ) ;
#7499 = ORIENTED_EDGE ( 'NONE', *, *, #4350, .F. ) ;
#7500 = VECTOR ( 'NONE', #2472, 1000.000000000000000 ) ;
#7501 = VERTEX_POINT ( 'NONE', #5282 ) ;
#7502 = DIRECTION ( 'NONE',  ( 0.000000000000000000, 0.000000000000000000, -1.000000000000000000 ) ) ;
#7503 = ADVANCED_FACE ( 'NONE', ( #4600 ), #354, .T. ) ;
#7504 = CARTESIAN_POINT ( 'NONE',  ( 384.0988265331048410, -18.06872101906905215, -8.580138959277956445 ) ) ;
#7505 = ORIENTED_EDGE ( 'NONE', *, *, #6623, .F. ) ;
#7506 = DIRECTION ( 'NONE',  ( 0.000000000000000000, -0.000000000000000000, -1.000000000000000000 ) ) ;
#7507 = CARTESIAN_POINT ( 'NONE',  ( 125.0000000000000000, 0.000000000000000000, 25.00000000000000000 ) ) ;
#7508 = DIRECTION ( 'NONE',  ( 0.000000000000000000, 0.000000000000000000, -1.000000000000000000 ) ) ;
#7510 = DIRECTION ( 'NONE',  ( 1.000000000000000000, 0.000000000000000000, 0.000000000000000000 ) ) ;
#7509 = AXIS2_PLACEMENT_3D ( 'NONE', #6761, #1268, #5361 ) ;
#7511 = CARTESIAN_POINT ( 'NONE',  ( 0.000000000000000000, 0.000000000000000000, 6.999999999999999112 ) ) ;
#7512 = ORIENTED_EDGE ( 'NONE', *, *, #4066, .T. ) ;
#7513 = AXIS2_PLACEMENT_3D ( 'NONE', #2139, #1617, #4019 ) ;
#7514 = EDGE_CURVE ( 'NONE', #4039, #1064, #915, .T. ) ;
#7515 = VERTEX_POINT ( 'NONE', #6494 ) ;
#7516 = FILL_AREA_STYLE ('',( #740 ) ) ;
#7517 = LINE ( 'NONE', #262, #3061 ) ;
#7518 = DIRECTION ( 'NONE',  ( 1.000000000000000000, 0.000000000000000000, 0.000000000000000000 ) ) ;
#7519 = CARTESIAN_POINT ( 'NONE',  ( 12.99038105676657651, -1.301042606982605321E-15, 7.500000000000000000 ) ) ;
#7520 = ORIENTED_EDGE ( 'NONE', *, *, #1932, .F. ) ;
#7521 = CIRCLE ( 'NONE', #4437, 0.5000000000000000000 ) ;
#7522 = EDGE_CURVE ( 'NONE', #5068, #6638, #6936, .T. ) ;
#7523 = VERTEX_POINT ( 'NONE', #836 ) ;
#7524 = TOROIDAL_SURFACE ( 'NONE', #6630, 13.00000000000000178, 0.5000000000000000000 ) ;
#7525 = EDGE_CURVE ( 'NONE', #3351, #3564, #2201, .T. ) ;
#7526 = DIRECTION ( 'NONE',  ( 0.000000000000000000, 0.000000000000000000, 1.000000000000000000 ) ) ;
#7527 = VERTEX_POINT ( 'NONE', #3450 ) ;
#7528 = CARTESIAN_POINT ( 'NONE',  ( 46.25000000000002842, 113.0000000000000426, 130.0000000000000000 ) ) ;
#7529 = VERTEX_POINT ( 'NONE', #7733 ) ;
#7530 = DIRECTION ( 'NONE',  ( 1.000000000000000000, 0.000000000000000000, 0.000000000000000000 ) ) ;
#7531 = CARTESIAN_POINT ( 'NONE',  ( 47.50000000000000711, 177.5000000000000000, 0.000000000000000000 ) ) ;
#7532 = CIRCLE ( 'NONE', #1124, 12.50000000000000355 ) ;
#7533 = ADVANCED_FACE ( 'NONE', ( #6974 ), #7667, .T. ) ;
#7534 = CONICAL_SURFACE ( 'NONE', #4072, 11.64999999999996660, 0.7853981633974482790 ) ;
#7535 = EDGE_CURVE ( 'NONE', #5833, #6373, #3364, .T. ) ;
#7536 = ORIENTED_EDGE ( 'NONE', *, *, #85, .T. ) ;
#7537 = DIRECTION ( 'NONE',  ( 0.000000000000000000, 0.000000000000000000, 1.000000000000000000 ) ) ;
#7538 = VERTEX_POINT ( 'NONE', #3999 ) ;
#7539 = VECTOR ( 'NONE', #3344, 1000.000000000000000 ) ;
#7540 = VECTOR ( 'NONE', #7163, 1000.000000000000227 ) ;
#7541 = VERTEX_POINT ( 'NONE', #6449 ) ;
#7542 = LINE ( 'NONE', #245, #1253 ) ;
#7543 = DIRECTION ( 'NONE',  ( 0.000000000000000000, 0.000000000000000000, 1.000000000000000000 ) ) ;
#7544 = CARTESIAN_POINT ( 'NONE',  ( 398.0000000000001137, 12.50000000000000000, -15.61249499599599488 ) ) ;
#7545 = ORIENTED_EDGE ( 'NONE', *, *, #7765, .F. ) ;
#7546 = DIRECTION ( 'NONE',  ( 1.000000000000000000, 0.000000000000000000, 0.000000000000000000 ) ) ;
#7547 = VECTOR ( 'NONE', #1175, 1000.000000000000000 ) ;
#7548 = VECTOR ( 'NONE', #6906, 1000.000000000000000 ) ;
#7549 = CARTESIAN_POINT ( 'NONE',  ( 0.000000000000000000, 0.000000000000000000, 0.000000000000000000 ) ) ;
#7550 = DIRECTION ( 'NONE',  ( 0.000000000000000000, -0.000000000000000000, 1.000000000000000000 ) ) ;
#7551 = CARTESIAN_POINT ( 'NONE',  ( 11.46392929283375928, -22.21662272193747256, 25.00000000000000000 ) ) ;
#7552 = DIRECTION ( 'NONE',  ( -1.000000000000000000, 0.000000000000000000, 0.000000000000000000 ) ) ;
#7553 = EDGE_CURVE ( 'NONE', #2350, #781, #2076, .T. ) ;
#7554 = ORIENTED_EDGE ( 'NONE', *, *, #6000, .T. ) ;
#7555 = DIRECTION ( 'NONE',  ( 4.789677997474691297E-16, -1.000000000000000000, 0.000000000000000000 ) ) ;
#7556 = DIRECTION ( 'NONE',  ( 0.9847062208914426629, -4.716425720178463790E-16, -0.1742230138003970086 ) ) ;
#7557 = ORIENTED_EDGE ( 'NONE', *, *, #2189, .T. ) ;
#7558 = FACE_OUTER_BOUND ( 'NONE', #6243, .T. ) ;
#7559 = CARTESIAN_POINT ( 'NONE',  ( 46.25000000000002842, 47.50000000000003553, 195.5000000000000000 ) ) ;
#7560 = LINE ( 'NONE', #2060, #2742 ) ;
#7561 = CARTESIAN_POINT ( 'NONE',  ( -12.50000000000000000, 0.000000000000000000, 6.999999999999999112 ) ) ;
#7562 = ORIENTED_EDGE ( 'NONE', *, *, #4625, .F. ) ;
#7563 = ADVANCED_BREP_SHAPE_REPRESENTATION ( '', ( #4361, #5785 ), #6420 ) ;
#7564 = VERTEX_POINT ( 'NONE', #875 ) ;
#7565 = DIRECTION ( 'NONE',  ( -4.789677997474686366E-16, -1.000000000000000000, -0.000000000000000000 ) ) ;
#7566 = VERTEX_POINT ( 'NONE', #3330 ) ;
#7567 = CARTESIAN_POINT ( 'NONE',  ( 150.0000000000000000, 1.836970198721029747E-14, 25.00000000000000000 ) ) ;
#7568 = DIRECTION ( 'NONE',  ( 0.000000000000000000, 0.000000000000000000, 1.000000000000000000 ) ) ;
#7569 = DIRECTION ( 'NONE',  ( -0.000000000000000000, 0.000000000000000000, 1.000000000000000000 ) ) ;
#7570 = FACE_OUTER_BOUND ( 'NONE', #6819, .T. ) ;
#7571 = EDGE_CURVE ( 'NONE', #5563, #905, #278, .T. ) ;
#7572 = ORIENTED_EDGE ( 'NONE', *, *, #1985, .F. ) ;
#7573 = CARTESIAN_POINT ( 'NONE',  ( 6.495190528383280260, 16.25000000000000000, 7.500000000000000000 ) ) ;
#7574 = ORIENTED_EDGE ( 'NONE', *, *, #7571, .F. ) ;
#7575 = EDGE_CURVE ( 'NONE', #107, #1830, #7613, .T. ) ;
#7576 = ORIENTED_EDGE ( 'NONE', *, *, #4211, .F. ) ;
#7577 = DIRECTION ( 'NONE',  ( 1.000000000000000000, 0.000000000000000000, 0.000000000000000000 ) ) ;
#7578 = ADVANCED_FACE ( 'NONE', ( #2115 ), #4560, .T. ) ;
#7579 = DIRECTION ( 'NONE',  ( -0.000000000000000000, 0.000000000000000000, 1.000000000000000000 ) ) ;
#7580 = LINE ( 'NONE', #6337, #359 ) ;
#7581 = DIRECTION ( 'NONE',  ( -1.000000000000000000, 0.000000000000000000, 0.000000000000000000 ) ) ;
#7582 = EDGE_CURVE ( 'NONE', #2766, #2146, #3452, .T. ) ;
#7583 = EDGE_LOOP ( 'NONE', ( #594, #1147 ) ) ;
#7584 = EDGE_CURVE ( 'NONE', #6578, #1942, #7298, .T. ) ;
#7585 = CARTESIAN_POINT ( 'NONE',  ( -12.99038105676657651, 1.734723475976807094E-15, 7.500000000000000000 ) ) ;
#7586 = DIRECTION ( 'NONE',  ( -0.000000000000000000, 0.000000000000000000, -1.000000000000000000 ) ) ;
#7587 = FACE_OUTER_BOUND ( 'NONE', #1681, .T. ) ;
#7588 = DIRECTION ( 'NONE',  ( 0.000000000000000000, -1.000000000000000000, -1.387778780781445676E-16 ) ) ;
#7589 = VERTEX_POINT ( 'NONE', #7886 ) ;
#7590 = FACE_BOUND ( 'NONE', #1902, .T. ) ;
#7591 =( NAMED_UNIT ( * ) PLANE_ANGLE_UNIT ( ) SI_UNIT ( $, .RADIAN. ) );
#7592 = ORIENTED_EDGE ( 'NONE', *, *, #6593, .F. ) ;
#7593 = CARTESIAN_POINT ( 'NONE',  ( 42.50000000000000000, 47.50000000000003553, 0.000000000000000000 ) ) ;
#7594 = LINE ( 'NONE', #4543, #106 ) ;
#7595 = PLANE ( 'NONE',  #1329 ) ;
#7596 = EDGE_CURVE ( 'NONE', #4834, #2321, #2844, .T. ) ;
#7597 = FACE_BOUND ( 'NONE', #2160, .T. ) ;
#7598 = ORIENTED_EDGE ( 'NONE', *, *, #5026, .F. ) ;
#7599 = PRODUCT_DEFINITION_CONTEXT ( 'detailed design', #549, 'design' ) ;
#7600 = CLOSED_SHELL ( 'NONE', ( #6735, #865, #3178, #7747, #2631, #1403, #4817, #2388, #1745, #4750, #903, #5448, #330, #1550, #5345, #4630, #2572, #3945, #2655, #6293, #6516, #528, #1709, #4823 ) ) ;
#7601 = ORIENTED_EDGE ( 'NONE', *, *, #6711, .T. ) ;
#7602 = CARTESIAN_POINT ( 'NONE',  ( 25.00000000000000000, 25.00000000000000000, 0.000000000000000000 ) ) ;
#7603 = EDGE_LOOP ( 'NONE', ( #6677, #2595, #7126, #7378 ) ) ;
#7604 = CARTESIAN_POINT ( 'NONE',  ( -26.24999999999997158, 47.50000000000009237, 17.50000000000001421 ) ) ;
#7605 = CARTESIAN_POINT ( 'NONE',  ( -27.49999999999989342, 177.4999999999999432, 12.65877081724072362 ) ) ;
#7606 = VECTOR ( 'NONE', #2831, 1000.000000000000000 ) ;
#7607 = PLANE ( 'NONE',  #6002 ) ;
#7608 = LINE ( 'NONE', #233, #5573 ) ;
#7609 = CIRCLE ( 'NONE', #2617, 12.50000000000000000 ) ;
#7610 = CIRCLE ( 'NONE', #57, 25.00000000000000711 ) ;
#7611 = ORIENTED_EDGE ( 'NONE', *, *, #2727, .F. ) ;
#7612 = VECTOR ( 'NONE', #692, 1000.000000000000000 ) ;
#7613 = LINE ( 'NONE', #5243, #4083 ) ;
#7614 = ORIENTED_EDGE ( 'NONE', *, *, #1103, .F. ) ;
#7615 = ORIENTED_EDGE ( 'NONE', *, *, #4107, .F. ) ;
#7616 = DIRECTION ( 'NONE',  ( 0.000000000000000000, -0.000000000000000000, -1.000000000000000000 ) ) ;
#7617 = CARTESIAN_POINT ( 'NONE',  ( 52.50000000000000711, 111.9999999999998863, 130.0000000000000000 ) ) ;
#7618 = EDGE_CURVE ( 'NONE', #5012, #268, #439, .T. ) ;
#7619 = CIRCLE ( 'NONE', #7120, 5.000000000000000888 ) ;
#7620 = VERTEX_POINT ( 'NONE', #1073 ) ;
#7621 = EDGE_CURVE ( 'NONE', #2387, #5237, #5632, .T. ) ;
#7622 = CARTESIAN_POINT ( 'NONE',  ( -10.82531754730547746, -13.74999999999999467, 0.000000000000000000 ) ) ;
#7623 = FACE_OUTER_BOUND ( 'NONE', #1039, .T. ) ;
#7624 = DIRECTION ( 'NONE',  ( 0.000000000000000000, 0.000000000000000000, 1.000000000000000000 ) ) ;
#7625 = DIRECTION ( 'NONE',  ( 1.000000000000000000, 0.000000000000000000, -0.000000000000000000 ) ) ;
#7626 = VECTOR ( 'NONE', #4959, 1000.000000000000000 ) ;
#7627 = CARTESIAN_POINT ( 'NONE',  ( 0.000000000000000000, 0.000000000000000000, 0.000000000000000000 ) ) ;
#7628 = DIRECTION ( 'NONE',  ( 0.000000000000000000, 0.000000000000000000, -1.000000000000000000 ) ) ;
#7629 = AXIS2_PLACEMENT_3D ( 'NONE', #6607, #3596, #6679 ) ;
#7630 = DIRECTION ( 'NONE',  ( -1.000000000000000000, 0.000000000000000000, -2.370375316168905181E-32 ) ) ;
#7631 = VERTEX_POINT ( 'NONE', #4238 ) ;
#7632 = LINE ( 'NONE', #2745, #7395 ) ;
#7633 = DIRECTION ( 'NONE',  ( -0.000000000000000000, 1.000000000000000000, 1.387778780781445676E-16 ) ) ;
#7634 = DIRECTION ( 'NONE',  ( -1.000000000000000000, 1.387778780781445676E-15, 0.000000000000000000 ) ) ;
#7635 = CARTESIAN_POINT ( 'NONE',  ( 17.50000000000000355, 2.143131898507868643E-15, 75.00000000000000000 ) ) ;
#7636 = ORIENTED_EDGE ( 'NONE', *, *, #5475, .F. ) ;
#7637 = PRODUCT_DEFINITION_SHAPE ( 'NONE', 'NONE',  #7923 ) ;
#7638 = ORIENTED_EDGE ( 'NONE', *, *, #3815, .T. ) ;
#7639 = EDGE_CURVE ( 'NONE', #3593, #4754, #1038, .T. ) ;
#7640 = PLANE ( 'NONE',  #3604 ) ;
#7641 = ORIENTED_EDGE ( 'NONE', *, *, #5819, .F. ) ;
#7642 = DIRECTION ( 'NONE',  ( 1.000000000000000000, 0.000000000000000000, 0.000000000000000000 ) ) ;
#7643 = VECTOR ( 'NONE', #5015, 1000.000000000000000 ) ;
#7644 = CARTESIAN_POINT ( 'NONE',  ( 41.66645320948619258, 47.44875693908029035, 12.50000000000000000 ) ) ;
#7645 = DIRECTION ( 'NONE',  ( -0.000000000000000000, 0.000000000000000000, 1.000000000000000000 ) ) ;
#7646 = CARTESIAN_POINT ( 'NONE',  ( 412.4999999999998295, 150.0000000000000284, 12.50000000000000000 ) ) ;
#7647 = CIRCLE ( 'NONE', #6123, 4.999999999999997335 ) ;
#7648 = EDGE_LOOP ( 'NONE', ( #5278, #635 ) ) ;
#7649 = DIRECTION ( 'NONE',  ( 1.000000000000000000, 0.000000000000000000, 0.000000000000000000 ) ) ;
#7650 = ORIENTED_EDGE ( 'NONE', *, *, #2984, .T. ) ;
#7651 = DIRECTION ( 'NONE',  ( 1.000000000000000000, 0.000000000000000000, 0.000000000000000000 ) ) ;
#7652 = ORIENTED_EDGE ( 'NONE', *, *, #3416, .T. ) ;
#7653 = DIRECTION ( 'NONE',  ( 0.000000000000000000, 0.000000000000000000, -1.000000000000000000 ) ) ;
#7654 = VECTOR ( 'NONE', #714, 1000.000000000000114 ) ;
#7655 = DIRECTION ( 'NONE',  ( -0.000000000000000000, -0.000000000000000000, -1.000000000000000000 ) ) ;
#7656 = LINE ( 'NONE', #6618, #2292 ) ;
#7657 = AXIS2_PLACEMENT_3D ( 'NONE', #6762, #701, #5518 ) ;
#7658 = CARTESIAN_POINT ( 'NONE',  ( 187.4999999999998863, 225.0000000000000284, 0.000000000000000000 ) ) ;
#7659 = ADVANCED_FACE ( 'NONE', ( #4158 ), #7848, .T. ) ;
#7660=STYLED_ITEM('',(#7969),#7024);
#7661 = CIRCLE ( 'NONE', #3824, 12.50000000000001066 ) ;
#7662 = ORIENTED_EDGE ( 'NONE', *, *, #6640, .T. ) ;
#7663 = DIRECTION ( 'NONE',  ( -0.000000000000000000, -0.000000000000000000, -1.000000000000000000 ) ) ;
#7664 = CARTESIAN_POINT ( 'NONE',  ( -37.49999999999989342, 187.4999999999999432, 12.50000000000000000 ) ) ;
#7665 = DIRECTION ( 'NONE',  ( -0.000000000000000000, 0.000000000000000000, 1.000000000000000000 ) ) ;
#7666 = CARTESIAN_POINT ( 'NONE',  ( 212.4999999999999147, 225.0000000000000284, 0.000000000000000000 ) ) ;
#7667 = TOROIDAL_SURFACE ( 'NONE', #3192, 15.00000000000000000, 5.000000000000000000 ) ;
#7668 = ADVANCED_FACE ( 'NONE', ( #1755 ), #1114, .T. ) ;
#7669 = VECTOR ( 'NONE', #534, 1000.000000000000000 ) ;
#7670 = CARTESIAN_POINT ( 'NONE',  ( 47.50000000000000711, 47.50000000000003553, 5.000000000000000000 ) ) ;
#7671 = EDGE_CURVE ( 'NONE', #1396, #6609, #2401, .T. ) ;
#7672 = DIRECTION ( 'NONE',  ( 1.000000000000000000, 0.000000000000000000, 0.000000000000000000 ) ) ;
#7673 = CIRCLE ( 'NONE', #6391, 12.50000000000000355 ) ;
#7674 = DIRECTION ( 'NONE',  ( -4.788861976295939431E-16, -0.9999999999999998890, -1.767773035661397189E-20 ) ) ;
#7675 = ORIENTED_EDGE ( 'NONE', *, *, #1888, .T. ) ;
#7676 =( NAMED_UNIT ( * ) SI_UNIT ( $, .STERADIAN. ) SOLID_ANGLE_UNIT ( ) );
#7677 = LINE ( 'NONE', #4582, #6515 ) ;
#7678 = CARTESIAN_POINT ( 'NONE',  ( 190.0000000000000000, -12.50000000000000000, 15.61249499599599488 ) ) ;
#7679 = EDGE_CURVE ( 'NONE', #2637, #2101, #6656, .T. ) ;
#7680 = DIRECTION ( 'NONE',  ( 1.000000000000000000, 0.000000000000000000, 0.000000000000000000 ) ) ;
#7681 = ORIENTED_EDGE ( 'NONE', *, *, #7525, .T. ) ;
#7682 = EDGE_CURVE ( 'NONE', #4500, #4609, #6572, .T. ) ;
#7683 = EDGE_LOOP ( 'NONE', ( #5378, #4759 ) ) ;
#7684 = FACE_BOUND ( 'NONE', #5316, .T. ) ;
#7685 = ORIENTED_EDGE ( 'NONE', *, *, #7487, .T. ) ;
#7686 = EDGE_CURVE ( 'NONE', #5527, #7541, #7673, .T. ) ;
#7687 = CARTESIAN_POINT ( 'NONE',  ( 326.6025403784437913, 75.00000000000005684, 125.0000000000000000 ) ) ;
#7688 = DIRECTION ( 'NONE',  ( -1.000000000000000000, -0.000000000000000000, -0.000000000000000000 ) ) ;
#7689 = ORIENTED_EDGE ( 'NONE', *, *, #5037, .T. ) ;
#7690 = SURFACE_SIDE_STYLE ('',( #5192 ) ) ;
#7691 = CARTESIAN_POINT ( 'NONE',  ( 46.25000000000002842, 177.5000000000000000, 17.50000000000001421 ) ) ;
#7692 = ORIENTED_EDGE ( 'NONE', *, *, #4491, .F. ) ;
#7693 = CARTESIAN_POINT ( 'NONE',  ( 38.21904415029502644, 62.70544120911855401, 12.50000000000000000 ) ) ;
#7695 = ORIENTED_EDGE ( 'NONE', *, *, #3562, .F. ) ;
#7694 = AXIS2_PLACEMENT_3D ( 'NONE', #3915, #6361, #3319 ) ;
#7696 = DIRECTION ( 'NONE',  ( -0.000000000000000000, 0.000000000000000000, 1.000000000000000000 ) ) ;
#7697 = ORIENTED_EDGE ( 'NONE', *, *, #2979, .T. ) ;
#7698 = CARTESIAN_POINT ( 'NONE',  ( 0.000000000000000000, 111.9999999999999858, 130.0000000000000000 ) ) ;
#7699 =( NAMED_UNIT ( * ) PLANE_ANGLE_UNIT ( ) SI_UNIT ( $, .RADIAN. ) );
#7700 = FACE_OUTER_BOUND ( 'NONE', #7840, .T. ) ;
#7701 = CARTESIAN_POINT ( 'NONE',  ( 52.50000000000000711, 177.5000000000000000, 5.000000000000000000 ) ) ;
#7702 = EDGE_CURVE ( 'NONE', #511, #6088, #5489, .T. ) ;
#7703 = ORIENTED_EDGE ( 'NONE', *, *, #6355, .F. ) ;
#7704 = PRODUCT ( 'Handle', 'Handle', '', ( #7354 ) ) ;
#7705 = PRODUCT_DEFINITION_FORMATION_WITH_SPECIFIED_SOURCE ( 'ANY', '', #1995, .NOT_KNOWN. ) ;
#7706 = CARTESIAN_POINT ( 'NONE',  ( 6.249999999999977796, 0.000000000000000000, 0.000000000000000000 ) ) ;
#7707 = LINE ( 'NONE', #5340, #5498 ) ;
#7708 = DIRECTION ( 'NONE',  ( 1.000000000000000000, 0.000000000000000000, 0.000000000000000000 ) ) ;
#7709 = DIRECTION ( 'NONE',  ( -0.000000000000000000, -0.000000000000000000, -1.000000000000000000 ) ) ;
#7710 = CARTESIAN_POINT ( 'NONE',  ( 387.0553328717124941, 19.72489609666084576, 3.330011984645298462 ) ) ;
#7711 = CARTESIAN_POINT ( 'NONE',  ( 398.0000000000001137, 12.50000000000000000, 15.61249499599599488 ) ) ;
#7712 =( NAMED_UNIT ( * ) PLANE_ANGLE_UNIT ( ) SI_UNIT ( $, .RADIAN. ) );
#7713 = ORIENTED_EDGE ( 'NONE', *, *, #5807, .F. ) ;
#7714 = DIRECTION ( 'NONE',  ( -0.5000000000000003331, 0.8660254037844383745, 0.000000000000000000 ) ) ;
#7715 = DIRECTION ( 'NONE',  ( 0.000000000000000000, 0.000000000000000000, 1.000000000000000000 ) ) ;
#7716 = DIRECTION ( 'NONE',  ( 0.000000000000000000, 0.000000000000000000, -1.000000000000000000 ) ) ;
#7717 = DIRECTION ( 'NONE',  ( -4.789677997474686366E-16, -1.000000000000000000, -0.000000000000000000 ) ) ;
#7718 = ORIENTED_EDGE ( 'NONE', *, *, #6686, .F. ) ;
#7719 =( REPRESENTATION_RELATIONSHIP ('NONE','NONE', #6292, #7467 ) REPRESENTATION_RELATIONSHIP_WITH_TRANSFORMATION ( #804 )SHAPE_REPRESENTATION_RELATIONSHIP( ) );
#7720 = ORIENTED_EDGE ( 'NONE', *, *, #6328, .T. ) ;
#7721 = EDGE_CURVE ( 'NONE', #7515, #5649, #5403, .T. ) ;
#7722 =( NAMED_UNIT ( * ) SI_UNIT ( $, .STERADIAN. ) SOLID_ANGLE_UNIT ( ) );
#7723 = ORIENTED_EDGE ( 'NONE', *, *, #4245, .T. ) ;
#7724 = FACE_OUTER_BOUND ( 'NONE', #4825, .T. ) ;
#7725 = CARTESIAN_POINT ( 'NONE',  ( -74.28095588234631919, -62.29455879088143888, 12.50000000000000000 ) ) ;
#7726 = EDGE_CURVE ( 'NONE', #2838, #5244, #3201, .T. ) ;
#7727 = ORIENTED_EDGE ( 'NONE', *, *, #3323, .F. ) ;
#7728 = CARTESIAN_POINT ( 'NONE',  ( 0.000000000000000000, 0.000000000000000000, 200.0000000000000000 ) ) ;
#7729 = ADVANCED_FACE ( 'NONE', ( #7814 ), #6654, .F. ) ;
#7730 = EDGE_CURVE ( 'NONE', #2977, #1036, #2891, .T. ) ;
#7731 = ORIENTED_EDGE ( 'NONE', *, *, #3219, .T. ) ;
#7732 = CIRCLE ( 'NONE', #4530, 12.49999999999999822 ) ;
#7733 = CARTESIAN_POINT ( 'NONE',  ( -61.78095584970497356, -62.29455879088143888, 0.000000000000000000 ) ) ;
#7734 = ORIENTED_EDGE ( 'NONE', *, *, #1795, .F. ) ;
#7735 = AXIS2_PLACEMENT_3D ( 'NONE', #3322, #6967, #5277 ) ;
#7736 = CYLINDRICAL_SURFACE ( 'NONE', #7766, 15.00000000000000000 ) ;
#7737 = ORIENTED_EDGE ( 'NONE', *, *, #1037, .T. ) ;
#7738 = CARTESIAN_POINT ( 'NONE',  ( 158.9591979875528409, 23.33951095074252891, 25.00000000000000000 ) ) ;
#7739 = CARTESIAN_POINT ( 'NONE',  ( 0.7190441666157093570, -30.59582893112819946, 12.50000000000000000 ) ) ;
#7740 = CARTESIAN_POINT ( 'NONE',  ( -15.64999999999999680, 0.000000000000000000, 195.9999999999999716 ) ) ;
#7741 = CARTESIAN_POINT ( 'NONE',  ( 6.602357126051254174E-16, 5.366506855898817567E-31, 0.000000000000000000 ) ) ;
#7742 = AXIS2_PLACEMENT_3D ( 'NONE', #7431, #1926, #6825 ) ;
#7743=STYLED_ITEM('',(#7969),#1383);
#7744 = VECTOR ( 'NONE', #2707, 1000.000000000000000 ) ;
#7745 = VERTEX_POINT ( 'NONE', #6093 ) ;
#7746 = ORIENTED_EDGE ( 'NONE', *, *, #6670, .T. ) ;
#7747 = ADVANCED_FACE ( 'NONE', ( #3050 ), #2360, .F. ) ;
#7748 = AXIS2_PLACEMENT_3D ( 'NONE', #6503, #3459, #2083 ) ;
#7749 = CIRCLE ( 'NONE', #4151, 5.000000000000000888 ) ;
#7750 = AXIS2_PLACEMENT_3D ( 'NONE', #6154, #2540, #7358 ) ;
#7751 = CARTESIAN_POINT ( 'NONE',  ( 12.50000000000000355, 0.000000000000000000, 0.000000000000000000 ) ) ;
#7752 = CARTESIAN_POINT ( 'NONE',  ( -25.00000000000000000, 1.530808498934191521E-15, 12.50000000000000000 ) ) ;
#7753 = LINE ( 'NONE', #7828, #3659 ) ;
#7754 = CYLINDRICAL_SURFACE ( 'NONE', #5297, 12.50000000000000000 ) ;
#7755 = DIRECTION ( 'NONE',  ( -0.000000000000000000, -0.000000000000000000, 1.000000000000000000 ) ) ;
#7756 = VECTOR ( 'NONE', #4394, 1000.000000000000000 ) ;
#7757 = DIRECTION ( 'NONE',  ( 0.000000000000000000, -1.000000000000000000, -0.000000000000000000 ) ) ;
#7758 = DIRECTION ( 'NONE',  ( -0.5305848225548643882, 2.540699436203256294E-16, -0.8476318458354563656 ) ) ;
#7759 = VERTEX_POINT ( 'NONE', #5930 ) ;
#7760 = DIRECTION ( 'NONE',  ( -1.000000000000000000, -0.000000000000000000, -0.000000000000000000 ) ) ;
#7761 = DIRECTION ( 'NONE',  ( 0.000000000000000000, 0.000000000000000000, 1.000000000000000000 ) ) ;
#7762 = DIRECTION ( 'NONE',  ( -0.000000000000000000, 1.000000000000000000, 1.387778780781445676E-16 ) ) ;
#7763 = DIRECTION ( 'NONE',  ( 1.000000000000000000, 0.000000000000000000, 0.000000000000000000 ) ) ;
#7764 = ORIENTED_EDGE ( 'NONE', *, *, #1065, .T. ) ;
#7765 = EDGE_CURVE ( 'NONE', #1377, #322, #2554, .T. ) ;
#7766 = AXIS2_PLACEMENT_3D ( 'NONE', #2249, #2893, #4680 ) ;
#7767 = ORIENTED_EDGE ( 'NONE', *, *, #1831, .T. ) ;
#7768 = ORIENTED_EDGE ( 'NONE', *, *, #3470, .T. ) ;
#7769 = DIRECTION ( 'NONE',  ( -0.000000000000000000, 1.000000000000000000, -0.000000000000000000 ) ) ;
#7770 = CARTESIAN_POINT ( 'NONE',  ( 325.0000000000000000, 12.50000000000000000, 25.00000000000000000 ) ) ;
#7771 = EDGE_LOOP ( 'NONE', ( #6296, #265, #181, #2018 ) ) ;
#7772 = CARTESIAN_POINT ( 'NONE',  ( 12.50000000000000000, 0.000000000000000000, 0.000000000000000000 ) ) ;
#7773 =( GEOMETRIC_REPRESENTATION_CONTEXT ( 3 ) GLOBAL_UNCERTAINTY_ASSIGNED_CONTEXT ( ( #2712 ) ) GLOBAL_UNIT_ASSIGNED_CONTEXT ( ( #7252, #551, #6082 ) ) REPRESENTATION_CONTEXT ( 'NONE', 'WORKASPACE' ) );
#7774 = CARTESIAN_POINT ( 'NONE',  ( 0.000000000000000000, 3.827021247335478113E-15, -31.24999999999999289 ) ) ;
#7775 = ADVANCED_FACE ( 'NONE', ( #7488 ), #2169, .T. ) ;
#7776 = EDGE_CURVE ( 'NONE', #3409, #968, #772, .T. ) ;
#7777 = ORIENTED_EDGE ( 'NONE', *, *, #5784, .T. ) ;
#7778 = VECTOR ( 'NONE', #3429, 1000.000000000000000 ) ;
#7779 = DIRECTION ( 'NONE',  ( 0.000000000000000000, 0.000000000000000000, 1.000000000000000000 ) ) ;
#7780 = VERTEX_POINT ( 'NONE', #5609 ) ;
#7781 = CARTESIAN_POINT ( 'NONE',  ( 52.50000000000000711, 144.7499999999999147, 130.0000000000000000 ) ) ;
#7782 = VERTEX_POINT ( 'NONE', #4353 ) ;
#7783 = DIRECTION ( 'NONE',  ( 1.000000000000000000, 0.000000000000000000, 0.000000000000000000 ) ) ;
#7784 = EDGE_CURVE ( 'NONE', #7541, #7529, #108, .T. ) ;
#7785 = DIRECTION ( 'NONE',  ( 0.000000000000000000, 0.000000000000000000, 1.000000000000000000 ) ) ;
#7786 = AXIS2_PLACEMENT_3D ( 'NONE', #6987, #4610, #5094 ) ;
#7787 = ORIENTED_EDGE ( 'NONE', *, *, #68, .T. ) ;
#7788 = ORIENTED_EDGE ( 'NONE', *, *, #3562, .T. ) ;
#7789 = CARTESIAN_POINT ( 'NONE',  ( 190.0000000000000000, 0.000000000000000000, 25.00000000000000000 ) ) ;
#7790 = ADVANCED_FACE ( 'NONE', ( #3126 ), #6809, .F. ) ;
#7791 = FACE_OUTER_BOUND ( 'NONE', #4591, .T. ) ;
#7792 = CARTESIAN_POINT ( 'NONE',  ( 10.49999999999999467, 0.000000000000000000, 0.000000000000000000 ) ) ;
#7793 = CARTESIAN_POINT ( 'NONE',  ( -37.49999999999995026, 37.50000000000010658, 12.50000000000000000 ) ) ;
#7794 = CARTESIAN_POINT ( 'NONE',  ( 375.0000000000000000, 15.61249499599599488, 12.50000000000000711 ) ) ;
#7795 = AXIS2_PLACEMENT_3D ( 'NONE', #6957, #1457, #5138 ) ;
#7796 = PLANE ( 'NONE',  #3944 ) ;
#7797 = VERTEX_POINT ( 'NONE', #6405 ) ;
#7798 = CIRCLE ( 'NONE', #1265, 31.25000000000000000 ) ;
#7799 = DIRECTION ( 'NONE',  ( 0.000000000000000000, 0.000000000000000000, 1.000000000000000000 ) ) ;
#7800 = LINE ( 'NONE', #5954, #5366 ) ;
#7801 = AXIS2_PLACEMENT_3D ( 'NONE', #5016, #2462, #4898 ) ;
#7802 = CARTESIAN_POINT ( 'NONE',  ( 0.000000000000000000, 0.000000000000000000, 25.00000000000000000 ) ) ;
#7803 = CARTESIAN_POINT ( 'NONE',  ( 0.000000000000000000, 0.000000000000000000, 6.999999999999999112 ) ) ;
#7804 = ORIENTED_EDGE ( 'NONE', *, *, #5576, .T. ) ;
#7805 = EDGE_CURVE ( 'NONE', #3051, #1999, #7005, .T. ) ;
#7806 = CIRCLE ( 'NONE', #5497, 65.50000000000000000 ) ;
#7807 = AXIS2_PLACEMENT_3D ( 'NONE', #1170, #3777, #6666 ) ;
#7808 = ORIENTED_EDGE ( 'NONE', *, *, #6261, .T. ) ;
#7809 = ORIENTED_EDGE ( 'NONE', *, *, #7045, .T. ) ;
#7810 = CYLINDRICAL_SURFACE ( 'NONE', #4556, 12.50000000000000000 ) ;
#7811 = FACE_BOUND ( 'NONE', #7403, .T. ) ;
#7812 = ORIENTED_EDGE ( 'NONE', *, *, #6468, .F. ) ;
#7813 = CARTESIAN_POINT ( 'NONE',  ( 0.000000000000000000, 2.678914873134841621E-15, 18.75000000000009948 ) ) ;
#7814 = FACE_OUTER_BOUND ( 'NONE', #367, .T. ) ;
#7815 = ORIENTED_EDGE ( 'NONE', *, *, #2999, .F. ) ;
#7816 = PRODUCT_RELATED_PRODUCT_CATEGORY ( 'part', '', ( #1621 ) ) ;
#7817 = CARTESIAN_POINT ( 'NONE',  ( -25.00000000000000000, 0.000000000000000000, 0.000000000000000000 ) ) ;
#7818 = VERTEX_POINT ( 'NONE', #7602 ) ;
#7819 = CARTESIAN_POINT ( 'NONE',  ( 296.6025403784439050, 87.50000000000005684, 12.50000000000000000 ) ) ;
#7820 = APPLICATION_CONTEXT ( 'automotive_design' ) ;
#7821 = EDGE_CURVE ( 'NONE', #7538, #6519, #4857, .T. ) ;
#7822 = DIRECTION ( 'NONE',  ( 0.000000000000000000, 1.000000000000000000, 0.000000000000000000 ) ) ;
#7823 = ORIENTED_EDGE ( 'NONE', *, *, #4989, .T. ) ;
#7824 = ORIENTED_EDGE ( 'NONE', *, *, #1027, .F. ) ;
#7825 = ADVANCED_FACE ( 'NONE', ( #7684, #5143 ), #2714, .T. ) ;
#7826 = CARTESIAN_POINT ( 'NONE',  ( 398.0000000000001137, -12.50000000000000000, -15.61249499599599488 ) ) ;
#7827 = FACE_BOUND ( 'NONE', #5965, .T. ) ;
#7828 = CARTESIAN_POINT ( 'NONE',  ( 286.6025403784437913, 0.000000000000000000, 0.000000000000000000 ) ) ;
#7829 = EDGE_CURVE ( 'NONE', #5920, #603, #3460, .T. ) ;
#7830 = CARTESIAN_POINT ( 'NONE',  ( -18.76388374866283471, 7.854341805648601650E-17, 0.000000000000000000 ) ) ;
#7831 = CARTESIAN_POINT ( 'NONE',  ( 386.1822627773321415, 19.20332549959546853, -5.601192942097885208 ) ) ;
#7832 = ADVANCED_FACE ( 'NONE', ( #2028 ), #5803, .T. ) ;
#7833 = ADVANCED_FACE ( 'NONE', ( #985 ), #2836, .F. ) ;
#7834 = CARTESIAN_POINT ( 'NONE',  ( -49.28095584970496645, 12.70544120911856112, 12.50000000000000000 ) ) ;
#7835 = APPLICATION_PROTOCOL_DEFINITION ( 'draft international standard', 'automotive_design', 1998, #549 ) ;
#7836 = LINE ( 'NONE', #3475, #5092 ) ;
#7837 = CARTESIAN_POINT ( 'NONE',  ( -26.66645320948613573, 47.44875693908033298, 12.50000000000000000 ) ) ;
#7838 = CARTESIAN_POINT ( 'NONE',  ( 15.64999999999999680, 1.916572240665607593E-15, 200.0000000000000000 ) ) ;
#7839 = VERTEX_POINT ( 'NONE', #267 ) ;
#7840 = EDGE_LOOP ( 'NONE', ( #2791, #7001, #6696, #390 ) ) ;
#7841 = SHAPE_REPRESENTATION_RELATIONSHIP ( 'NONE' , 'NONE' ,  #3730, #10 ) ;
#7842 = VERTEX_POINT ( 'NONE', #5072 ) ;
#7843 = ADVANCED_FACE ( 'NONE', ( #2636, #2756 ), #7640, .F. ) ;
#7844 = DIRECTION ( 'NONE',  ( 0.000000000000000000, -1.000000000000000000, 0.000000000000000000 ) ) ;
#7845 = ORIENTED_EDGE ( 'NONE', *, *, #3899, .T. ) ;
#7846 = CYLINDRICAL_SURFACE ( 'NONE', #2257, 12.50000000000001066 ) ;
#7847 = ORIENTED_EDGE ( 'NONE', *, *, #7394, .F. ) ;
#7848 = CYLINDRICAL_SURFACE ( 'NONE', #512, 65.50000000000000000 ) ;
#7849 = VERTEX_POINT ( 'NONE', #5232 ) ;
#7850 = CARTESIAN_POINT ( 'NONE',  ( 374.5751407255119716, -15.61249499599599666, -12.50000000000000000 ) ) ;
#7851 = ORIENTED_EDGE ( 'NONE', *, *, #3554, .F. ) ;
#7852 = FACE_BOUND ( 'NONE', #5070, .T. ) ;
#7853 = DIRECTION ( 'NONE',  ( -0.000000000000000000, -0.000000000000000000, -1.000000000000000000 ) ) ;
#7854 = ORIENTED_EDGE ( 'NONE', *, *, #7582, .F. ) ;
#7855 = VECTOR ( 'NONE', #1150, 1000.000000000000000 ) ;
#7856 = ORIENTED_EDGE ( 'NONE', *, *, #960, .T. ) ;
#7857 = CARTESIAN_POINT ( 'NONE',  ( 0.000000000000000000, 0.000000000000000000, 12.50000000000000000 ) ) ;
#7858 = LINE ( 'NONE', #4808, #3049 ) ;
#7859 = DIRECTION ( 'NONE',  ( 0.000000000000000000, 0.000000000000000000, -1.000000000000000000 ) ) ;
#7860 = DIRECTION ( 'NONE',  ( -0.000000000000000000, -0.000000000000000000, -1.000000000000000000 ) ) ;
#7861 = AXIS2_PLACEMENT_3D ( 'NONE', #2870, #1139, #5390 ) ;
#7862 = LINE ( 'NONE', #3621, #942 ) ;
#7863 = DIRECTION ( 'NONE',  ( 1.000000000000000000, 0.000000000000000000, 0.000000000000000000 ) ) ;
#7864 = EDGE_CURVE ( 'NONE', #7362, #3389, #908, .T. ) ;
#7865 = EDGE_CURVE ( 'NONE', #1918, #7015, #6321, .T. ) ;
#7866 = VECTOR ( 'NONE', #3224, 1000.000000000000000 ) ;
#7867 = LINE ( 'NONE', #582, #5370 ) ;
#7868 = CARTESIAN_POINT ( 'NONE',  ( 0.000000000000000000, 25.00000000000000000, 25.00000000000000000 ) ) ;
#7869 = CARTESIAN_POINT ( 'NONE',  ( 9.381941874331406694, 16.25000000000000000, 0.000000000000000000 ) ) ;
#7870 = DIRECTION ( 'NONE',  ( 0.000000000000000000, 0.000000000000000000, 1.000000000000000000 ) ) ;
#7871 = ORIENTED_EDGE ( 'NONE', *, *, #6261, .F. ) ;
#7872 = AXIS2_PLACEMENT_3D ( 'NONE', #7741, #2254, #446 ) ;
#7873 = CIRCLE ( 'NONE', #4409, 15.00000000000000000 ) ;
#7874 = ORIENTED_EDGE ( 'NONE', *, *, #6012, .F. ) ;
#7875 = VECTOR ( 'NONE', #5465, 1000.000000000000000 ) ;
#7876 = SHAPE_REPRESENTATION_RELATIONSHIP ( 'NONE' , 'NONE' ,  #444, #7563 ) ;
#7877 = EDGE_LOOP ( 'NONE', ( #1152, #3082, #7650, #6416 ) ) ;
#7878 = DIRECTION ( 'NONE',  ( 0.000000000000000000, 0.000000000000000000, -1.000000000000000000 ) ) ;
#7879 = FACE_OUTER_BOUND ( 'NONE', #5136, .T. ) ;
#7880 = FACE_BOUND ( 'NONE', #6724, .T. ) ;
#7881 = ORIENTED_EDGE ( 'NONE', *, *, #5936, .T. ) ;
#7882 = DIRECTION ( 'NONE',  ( 1.000000000000000000, 0.000000000000000000, 0.000000000000000000 ) ) ;
#7883 = AXIS2_PLACEMENT_3D ( 'NONE', #7567, #4513, #6364 ) ;
#7884 = EDGE_CURVE ( 'NONE', #7266, #3363, #4551, .T. ) ;
#7885 = ORIENTED_EDGE ( 'NONE', *, *, #4321, .F. ) ;
#7886 = CARTESIAN_POINT ( 'NONE',  ( 296.6025403784439050, 142.5000000000000000, 125.0000000000000000 ) ) ;
#7887 = VERTEX_POINT ( 'NONE', #3954 ) ;
#7888 = CARTESIAN_POINT ( 'NONE',  ( 373.3039311335094794, -15.69870025322426699, -12.39168528959425331 ) ) ;
#7889 = COLOUR_RGB ( '',0.7921568627450980005, 0.8196078431372548767, 0.9333333333333333481 ) ;
#7890 = ORIENTED_EDGE ( 'NONE', *, *, #6746, .T. ) ;
#7891 = CARTESIAN_POINT ( 'NONE',  ( 12.50000000000000000, 1.530808498934191521E-15, 0.000000000000000000 ) ) ;
#7892 = CARTESIAN_POINT ( 'NONE',  ( -27.49999999999994671, 37.50000000000008527, 12.50000000000000000 ) ) ;
#7893 = EDGE_CURVE ( 'NONE', #7188, #7382, #1928, .T. ) ;
#7894 = VERTEX_POINT ( 'NONE', #7083 ) ;
#7895 = ORIENTED_EDGE ( 'NONE', *, *, #3997, .F. ) ;
#7896 = CARTESIAN_POINT ( 'NONE',  ( 381.3155148028032499, -16.83062759343247805, 10.81672997705310557 ) ) ;
#7897 = CARTESIAN_POINT ( 'NONE',  ( 0.000000000000000000, 0.000000000000000000, 0.000000000000000000 ) ) ;
#7898 = DIRECTION ( 'NONE',  ( -0.000000000000000000, -0.000000000000000000, -1.000000000000000000 ) ) ;
#7900 = CARTESIAN_POINT ( 'NONE',  ( -37.49999999999994316, 225.0000000000000284, 12.50000000000000000 ) ) ;
#7899 = CIRCLE ( 'NONE', #5474, 5.000000000000000000 ) ;
#7901 = B_SPLINE_CURVE_WITH_KNOTS ( 'NONE', 3,
 ( #763, #122, #160, #2568, #6864, #3215, #3064, #5660, #682, #4973, #2606, #7504, #3138, #1923, #4290, #7388, #2002, #725, #1404, #6741, #6905, #611, #1247, #3704, #5538, #3744, #2492, #4932, #4326, #4365, #6822, #1323, #3020, #3743, #5536, #1168, #3101, #570, #610, #7896, #3616, #6183, #2370, #681, #3137, #2413, #37, #6026, #3, #4807 ),
 .UNSPECIFIED., .F., .F.,
 ( 4, 2, 2, 2, 2, 2, 2, 2, 2, 2, 2, 2, 2, 2, 2, 2, 2, 2, 2, 2, 2, 2, 2, 2, 4 ),
 ( 0.000000000000000000, 0.002511627799209755017, 0.003767441698814711672, 0.005023255598419669628, 0.007534883397629582938, 0.01004651119683949712, 0.01130232509644451058, 0.01255813899604952405, 0.01506976679525946078, 0.01632558069486442914, 0.01758139459446940098, 0.02009302239367936893, 0.02134883629328435117, 0.02260465019288934035, 0.02386046409249432260, 0.02511627799209930484, 0.02762790579130921381, 0.03013953359051911585, 0.03139534749012407033, 0.03265116138972902482, 0.03516278918893894073, 0.03641860308854381889, 0.03767441698814869705, 0.03893023088775358215, 0.04018604478735846031 ),
 .UNSPECIFIED. ) ;
#7902 = DIRECTION ( 'NONE',  ( 0.000000000000000000, 1.000000000000000000, 0.000000000000000000 ) ) ;
#7903 = CARTESIAN_POINT ( 'NONE',  ( 378.3244348223507245, 15.95794361973645792, -12.05683462702026176 ) ) ;
#7904 = AXIS2_PLACEMENT_3D ( 'NONE', #5501, #1765, #1246 ) ;
#7905 = DIRECTION ( 'NONE',  ( -0.000000000000000000, -0.000000000000000000, -1.000000000000000000 ) ) ;
#7906 = PRODUCT_DEFINITION ( 'UNKNOWN', '', #6171, #2960 ) ;
#7907 = DIRECTION ( 'NONE',  ( -1.000000000000000000, 0.000000000000000000, 0.000000000000000000 ) ) ;
#7908 = DIRECTION ( 'NONE',  ( 1.000000000000000000, 0.000000000000000000, 0.000000000000000000 ) ) ;
#7909 = DIRECTION ( 'NONE',  ( 0.000000000000000000, -0.000000000000000000, -1.000000000000000000 ) ) ;
#7910 = AXIS2_PLACEMENT_3D ( 'NONE', #3494, #2935, #6576 ) ;
#7911 = CIRCLE ( 'NONE', #2795, 37.50000000000000711 ) ;
#7912 = EDGE_CURVE ( 'NONE', #6044, #4483, #6676, .T. ) ;
#7913 = VERTEX_POINT ( 'NONE', #6484 ) ;
#7914 = AXIS2_PLACEMENT_3D ( 'NONE', #1632, #2885, #4596 ) ;
#7915 = VECTOR ( 'NONE', #2869, 1000.000000000000000 ) ;
#7916 = ORIENTED_EDGE ( 'NONE', *, *, #168, .F. ) ;
#7917 = NEXT_ASSEMBLY_USAGE_OCCURRENCE ( 'NAUO1', ' ', ' ', #4475, #7906, $ ) ;
#7918 = NEXT_ASSEMBLY_USAGE_OCCURRENCE ( 'NAUO2', ' ', ' ', #4475, #1877, $ ) ;
#7919 = NEXT_ASSEMBLY_USAGE_OCCURRENCE ( 'NAUO3', ' ', ' ', #4475, #7468, $ ) ;
#7920 = NEXT_ASSEMBLY_USAGE_OCCURRENCE ( 'NAUO4', ' ', ' ', #4475, #2123, $ ) ;
#7921 = NEXT_ASSEMBLY_USAGE_OCCURRENCE ( 'NAUO5', ' ', ' ', #4475, #3552, $ ) ;
#7922 = NEXT_ASSEMBLY_USAGE_OCCURRENCE ( 'NAUO6', ' ', ' ', #4475, #3304, $ ) ;
#7923 = NEXT_ASSEMBLY_USAGE_OCCURRENCE ( 'NAUO7', ' ', ' ', #4475, #4720, $ ) ;
#7924 = NEXT_ASSEMBLY_USAGE_OCCURRENCE ( 'NAUO8', ' ', ' ', #4475, #3552, $ ) ;
#7925 = NEXT_ASSEMBLY_USAGE_OCCURRENCE ( 'NAUO9', ' ', ' ', #4475, #1294, $ ) ;
#7926 = NEXT_ASSEMBLY_USAGE_OCCURRENCE ( 'NAUO10', ' ', ' ', #4475, #6885, $ ) ;
#7927 = NEXT_ASSEMBLY_USAGE_OCCURRENCE ( 'NAUO11', ' ', ' ', #4475, #1538, $ ) ;
#7928 = NEXT_ASSEMBLY_USAGE_OCCURRENCE ( 'NAUO12', ' ', ' ', #4475, #2231, $ ) ;
#7929 = NEXT_ASSEMBLY_USAGE_OCCURRENCE ( 'NAUO13', ' ', ' ', #4475, #6885, $ ) ;
#7930 = NEXT_ASSEMBLY_USAGE_OCCURRENCE ( 'NAUO14', ' ', ' ', #4475, #6885, $ ) ;
#7931 = NEXT_ASSEMBLY_USAGE_OCCURRENCE ( 'NAUO15', ' ', ' ', #4475, #2231, $ ) ;
#7932 = NEXT_ASSEMBLY_USAGE_OCCURRENCE ( 'NAUO16', ' ', ' ', #4475, #2231, $ ) ;
#7933 = NEXT_ASSEMBLY_USAGE_OCCURRENCE ( 'NAUO17', ' ', ' ', #4475, #2231, $ ) ;
#7934 = NEXT_ASSEMBLY_USAGE_OCCURRENCE ( 'NAUO18', ' ', ' ', #4475, #2231, $ ) ;
#7935=COLOUR_RGB('Dark Blue',0.08,0.2,0.34);
#7936=FILL_AREA_STYLE_COLOUR('',#7935);
#7937=FILL_AREA_STYLE('',(#7936));
#7938=SURFACE_STYLE_FILL_AREA(#7937);
#7939=SURFACE_SIDE_STYLE('',(#7938));
#7940=SURFACE_STYLE_USAGE(.BOTH.,#7939);
#7941=PRESENTATION_STYLE_ASSIGNMENT((#7940));
#7942=COLOUR_RGB('Light Blue',0.38,0.62,0.78);
#7943=FILL_AREA_STYLE_COLOUR('',#7942);
#7944=FILL_AREA_STYLE('',(#7943));
#7945=SURFACE_STYLE_FILL_AREA(#7944);
#7946=SURFACE_SIDE_STYLE('',(#7945));
#7947=SURFACE_STYLE_USAGE(.BOTH.,#7946);
#7948=PRESENTATION_STYLE_ASSIGNMENT((#7947));
#7949=COLOUR_RGB('Sky Blue',0.24,0.69,0.87);
#7950=FILL_AREA_STYLE_COLOUR('',#7949);
#7951=FILL_AREA_STYLE('',(#7950));
#7952=SURFACE_STYLE_FILL_AREA(#7951);
#7953=SURFACE_SIDE_STYLE('',(#7952));
#7954=SURFACE_STYLE_USAGE(.BOTH.,#7953);
#7955=PRESENTATION_STYLE_ASSIGNMENT((#7954));
#7956=COLOUR_RGB('Grey',0.48,0.52,0.57);
#7957=FILL_AREA_STYLE_COLOUR('',#7956);
#7958=FILL_AREA_STYLE('',(#7957));
#7959=SURFACE_STYLE_FILL_AREA(#7958);
#7960=SURFACE_SIDE_STYLE('',(#7959));
#7961=SURFACE_STYLE_USAGE(.BOTH.,#7960);
#7962=PRESENTATION_STYLE_ASSIGNMENT((#7961));
#7963=COLOUR_RGB('Black',0.12,0.14,0.17);
#7964=FILL_AREA_STYLE_COLOUR('',#7963);
#7965=FILL_AREA_STYLE('',(#7964));
#7966=SURFACE_STYLE_FILL_AREA(#7965);
#7967=SURFACE_SIDE_STYLE('',(#7966));
#7968=SURFACE_STYLE_USAGE(.BOTH.,#7967);
#7969=PRESENTATION_STYLE_ASSIGNMENT((#7968));
#7970=COLOUR_RGB('Off White',0.89,0.88,0.83);
#7971=FILL_AREA_STYLE_COLOUR('',#7970);
#7972=FILL_AREA_STYLE('',(#7971));
#7973=SURFACE_STYLE_FILL_AREA(#7972);
#7974=SURFACE_SIDE_STYLE('',(#7973));
#7975=SURFACE_STYLE_USAGE(.BOTH.,#7974);
#7976=PRESENTATION_STYLE_ASSIGNMENT((#7975));
ENDSEC;
END-ISO-10303-21;
